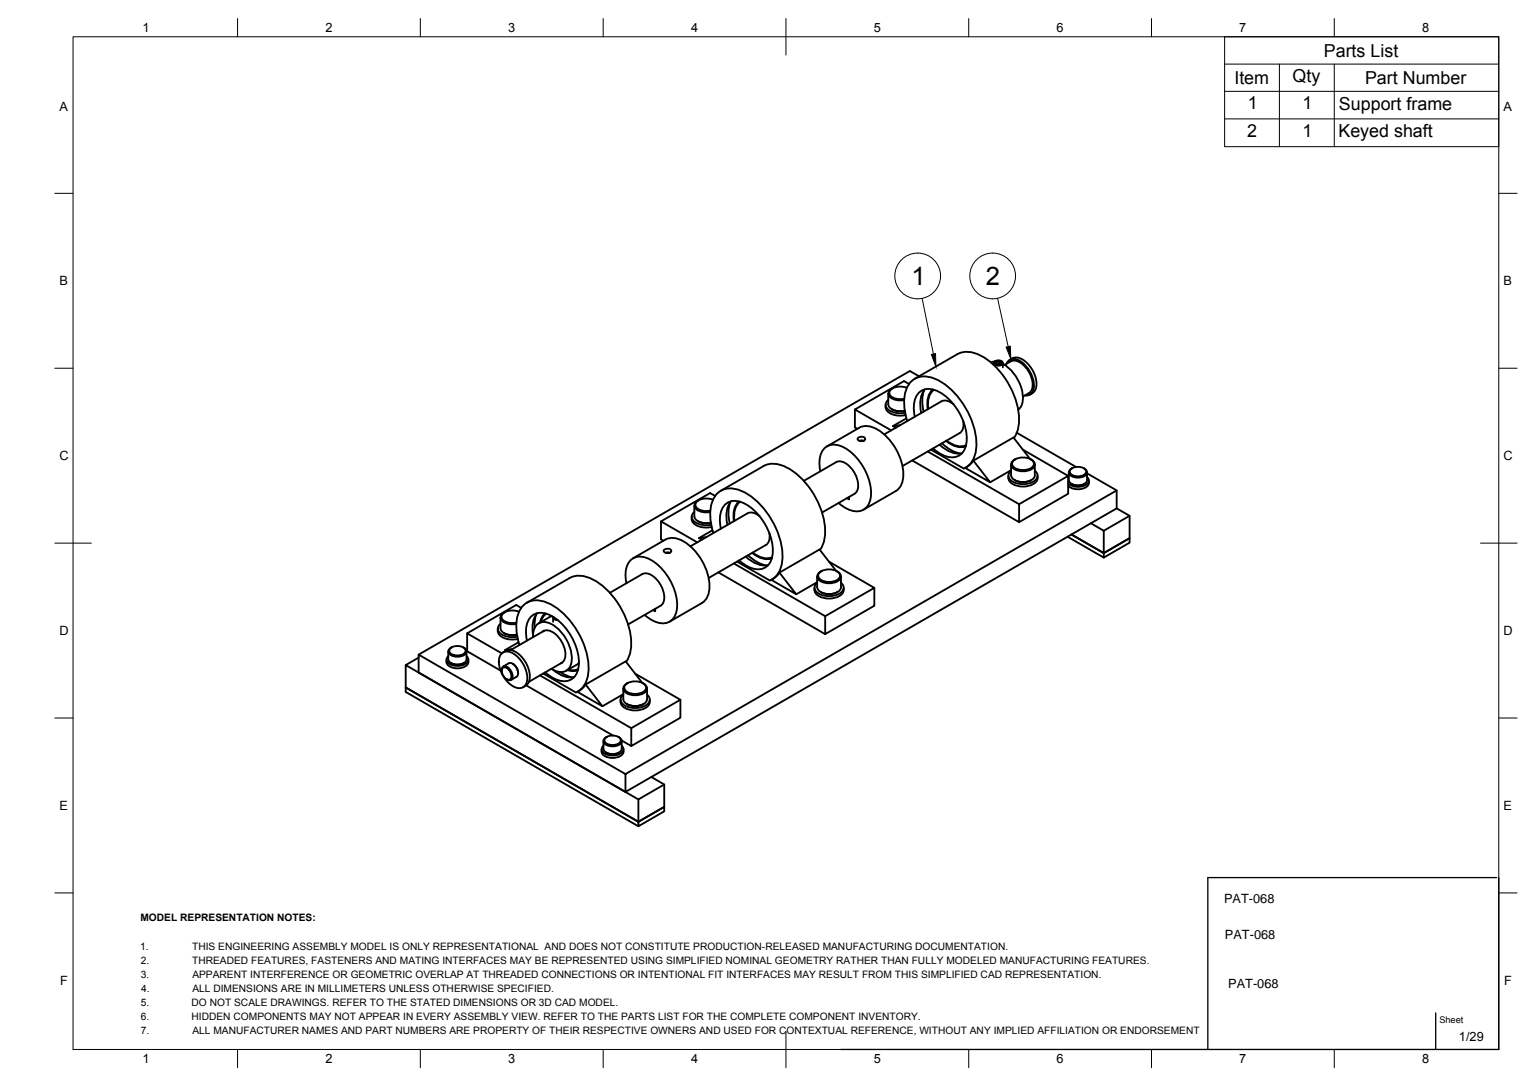
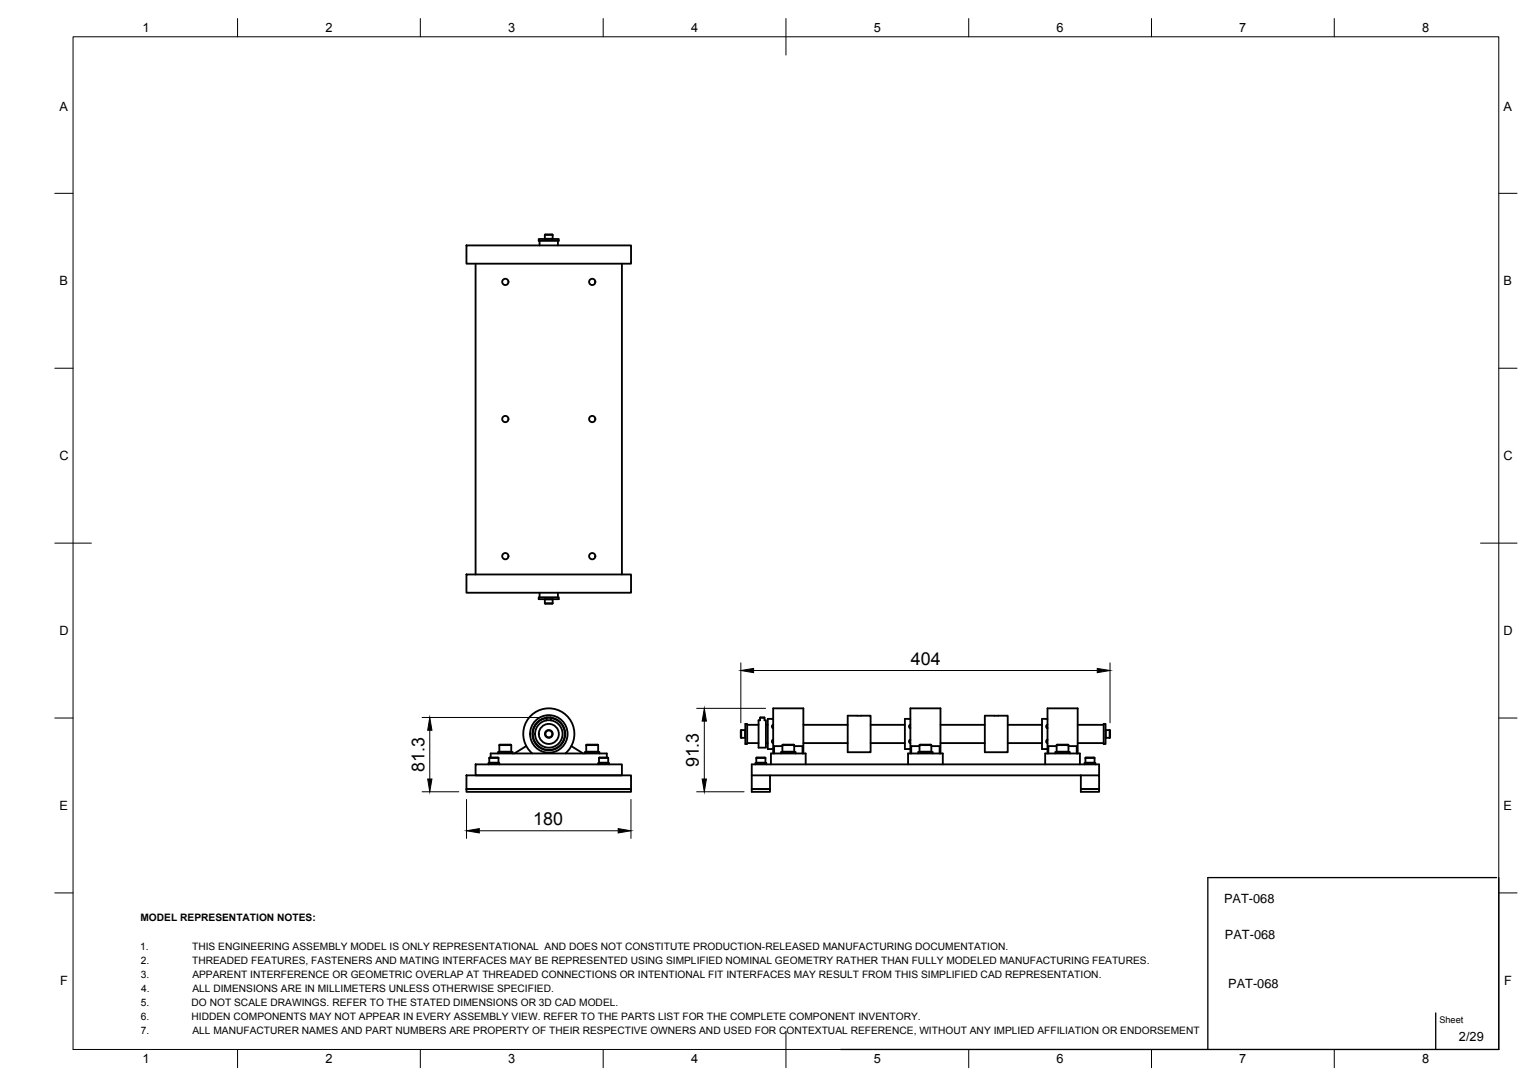
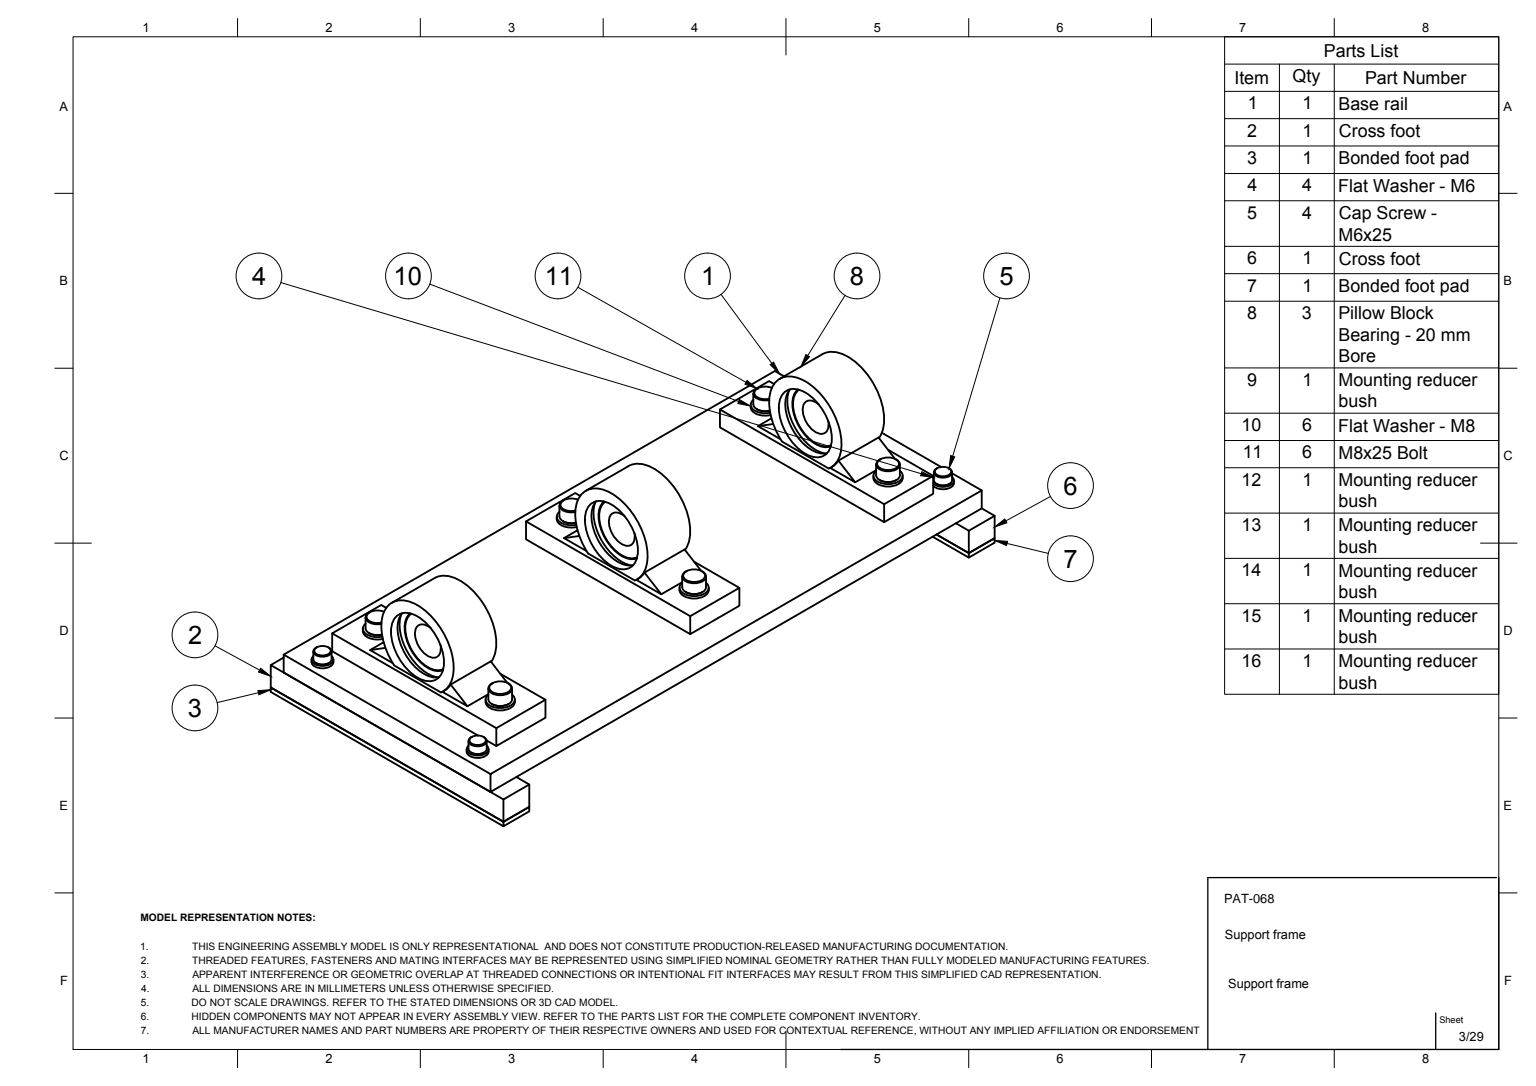
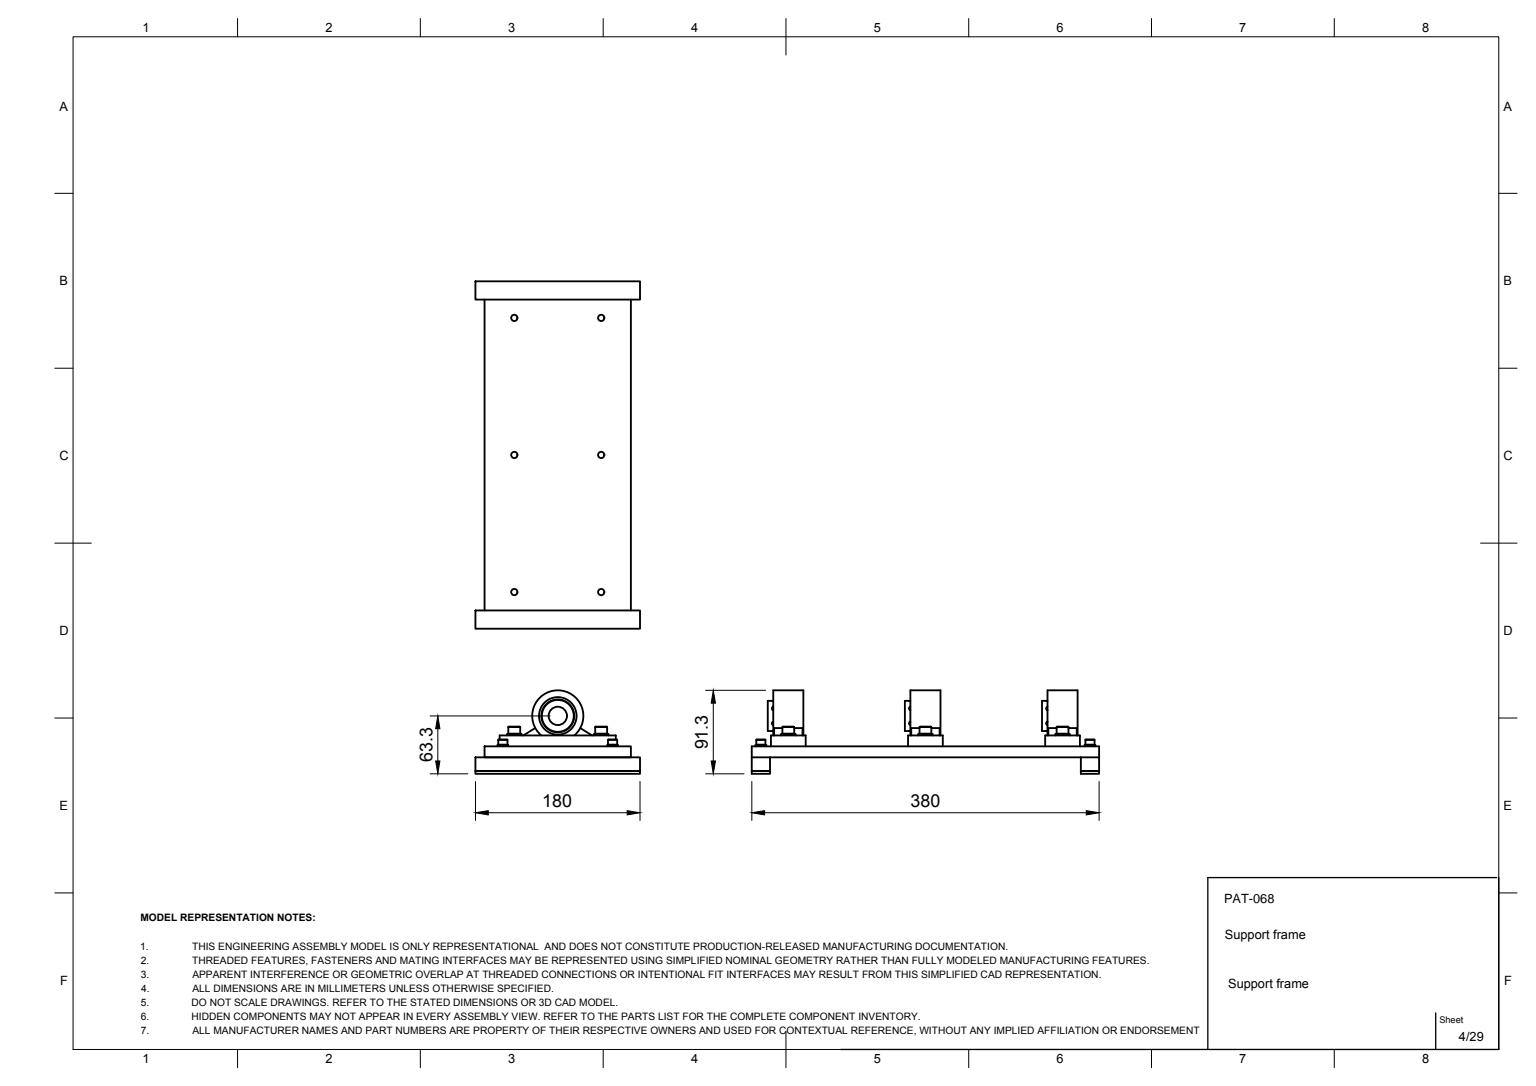
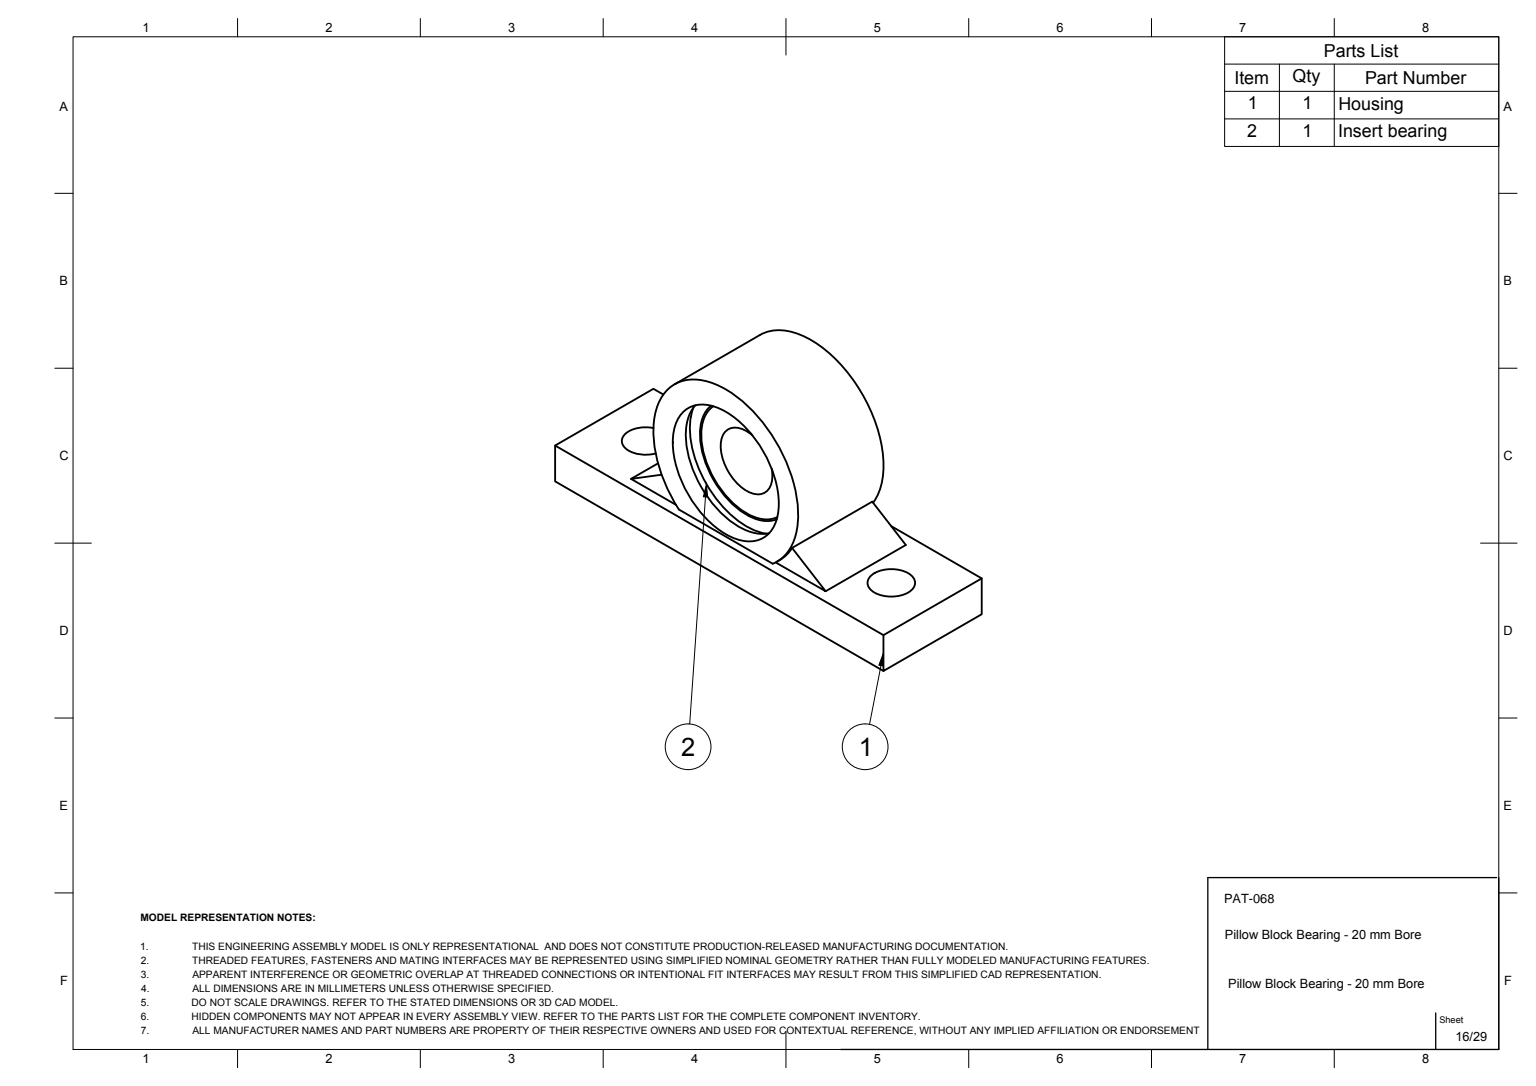
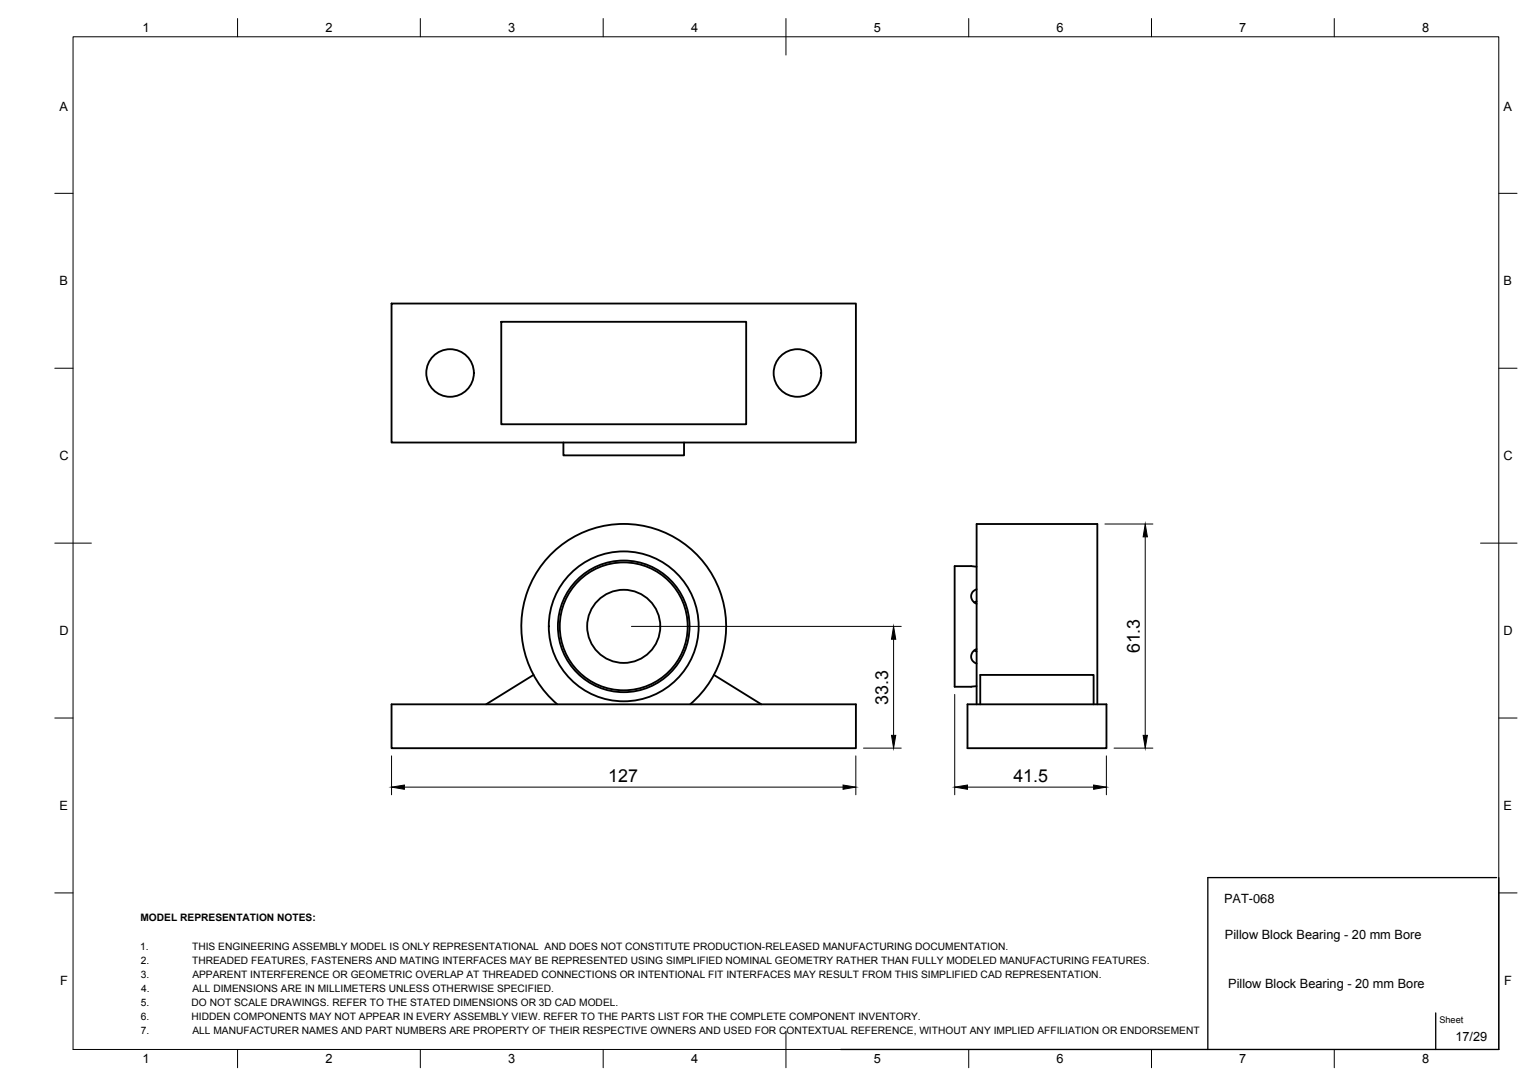
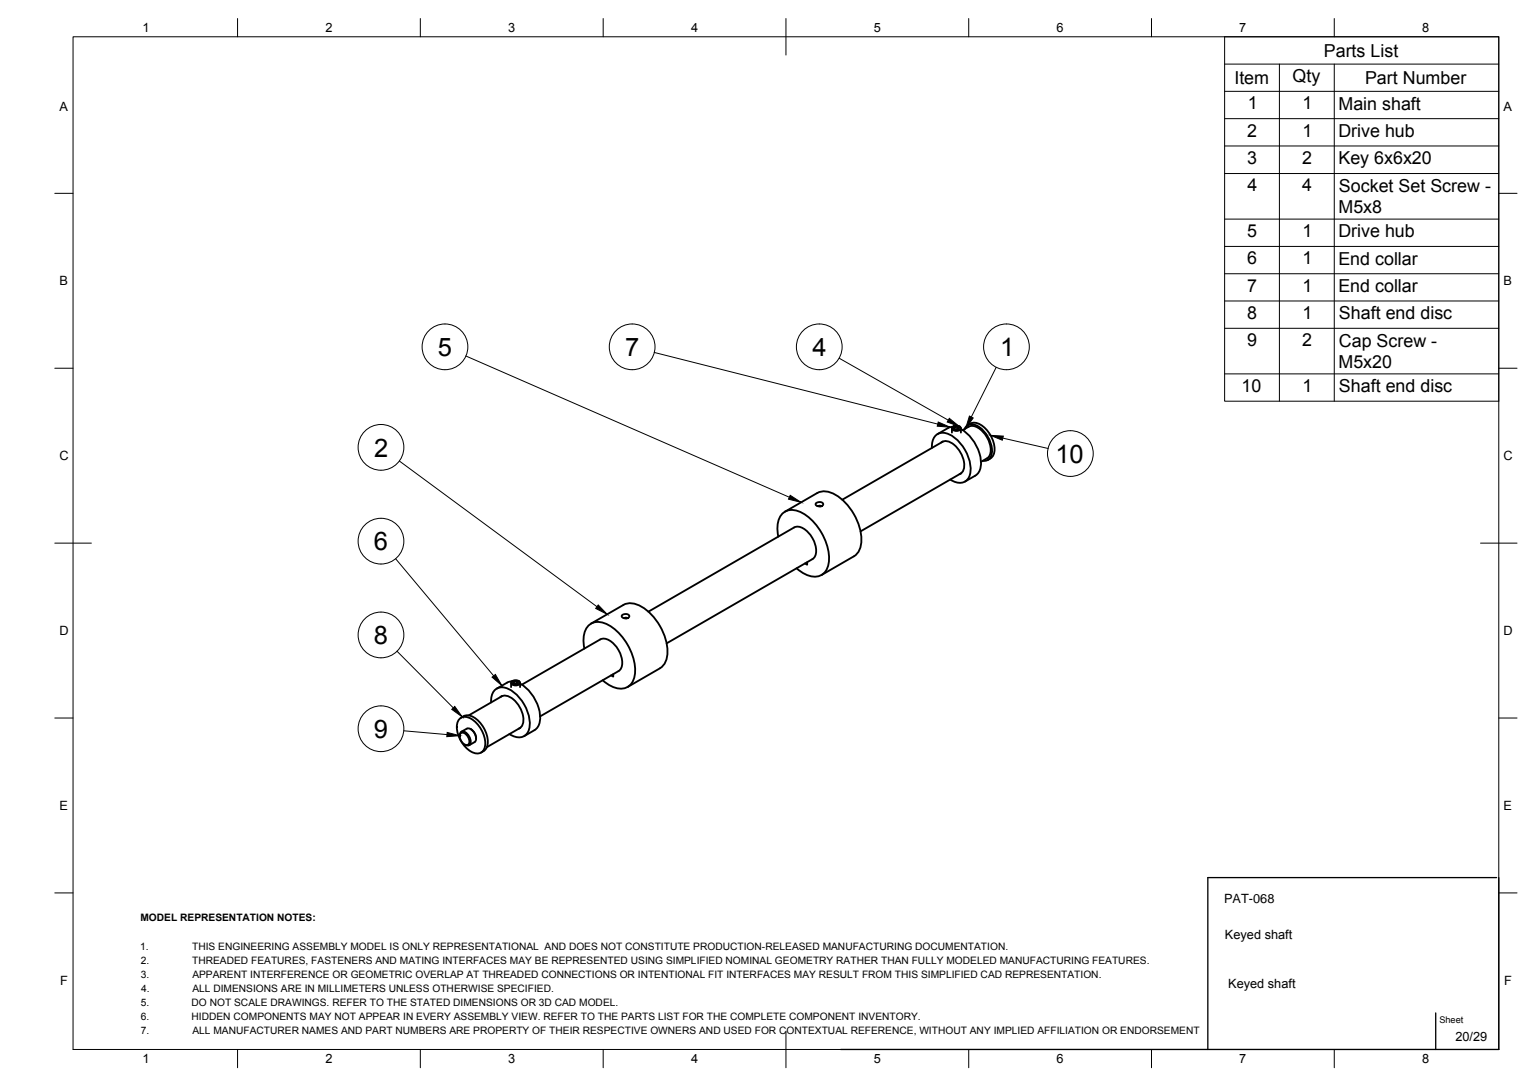
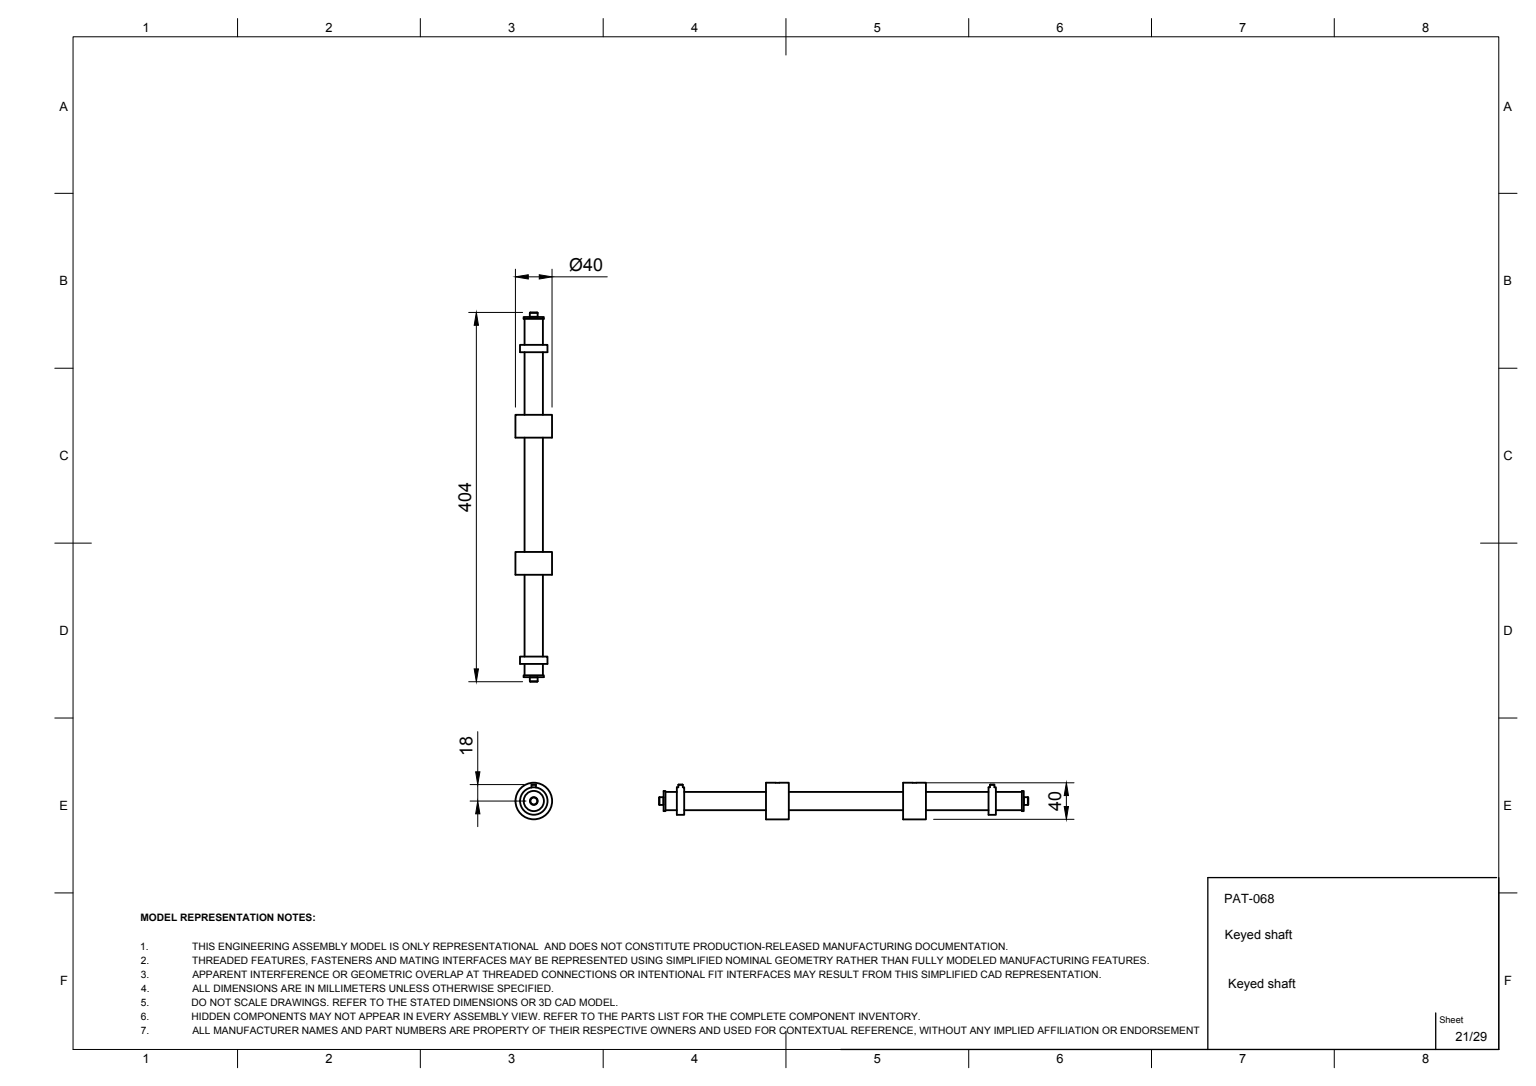
ISO-10303-21;
HEADER;
/* Generated by software containing ST-Developer
 * from STEP Tools, Inc. (www.steptools.com) 
 */

FILE_DESCRIPTION(
/* description */ ('Line shaft on three pillow blocks'),
/* implementation_level */ '2;1');

FILE_NAME(
/* name */ 'PAT-068',
/* time_stamp */ '2026-10-27T10:49:19-07:00',
/* author */ (''),
/* organization */ (''),
/* preprocessor_version */ 'ST-DEVELOPER v20.2',
/* originating_system */ 'Autodesk Translation Framework v15.17.0.0',
/* authorisation */ '');

FILE_SCHEMA (('AUTOMOTIVE_DESIGN { 1 0 10303 214 3 1 1 }'));
ENDSEC;

DATA;
#10=MECHANICAL_DESIGN_GEOMETRIC_PRESENTATION_REPRESENTATION('',(#338,#339,
#340,#341,#342,#343,#344,#345,#346,#347,#348,#349,#350,#351,#352,#353,#354,
#355,#356,#357,#358,#359,#360,#361,#362,#363,#364,#365),#8377);
#11=ITEM_DEFINED_TRANSFORMATION($,$,#4826,#4895);
#12=ITEM_DEFINED_TRANSFORMATION($,$,#4867,#4896);
#13=ITEM_DEFINED_TRANSFORMATION($,$,#4655,#4930);
#14=ITEM_DEFINED_TRANSFORMATION($,$,#4692,#4931);
#15=ITEM_DEFINED_TRANSFORMATION($,$,#4707,#4932);
#16=ITEM_DEFINED_TRANSFORMATION($,$,#4714,#4933);
#17=ITEM_DEFINED_TRANSFORMATION($,$,#4729,#4934);
#18=ITEM_DEFINED_TRANSFORMATION($,$,#4736,#4935);
#19=ITEM_DEFINED_TRANSFORMATION($,$,#4745,#4936);
#20=ITEM_DEFINED_TRANSFORMATION($,$,#4754,#4937);
#21=ITEM_DEFINED_TRANSFORMATION($,$,#4763,#4938);
#22=ITEM_DEFINED_TRANSFORMATION($,$,#4772,#4939);
#23=ITEM_DEFINED_TRANSFORMATION($,$,#4781,#4940);
#24=ITEM_DEFINED_TRANSFORMATION($,$,#4790,#4941);
#25=ITEM_DEFINED_TRANSFORMATION($,$,#4799,#4942);
#26=ITEM_DEFINED_TRANSFORMATION($,$,#4790,#4943);
#27=ITEM_DEFINED_TRANSFORMATION($,$,#4799,#4944);
#28=ITEM_DEFINED_TRANSFORMATION($,$,#4790,#4945);
#29=ITEM_DEFINED_TRANSFORMATION($,$,#4799,#4946);
#30=ITEM_DEFINED_TRANSFORMATION($,$,#4790,#4947);
#31=ITEM_DEFINED_TRANSFORMATION($,$,#4799,#4948);
#32=ITEM_DEFINED_TRANSFORMATION($,$,#4825,#4949);
#33=ITEM_DEFINED_TRANSFORMATION($,$,#4897,#4950);
#34=ITEM_DEFINED_TRANSFORMATION($,$,#4906,#4951);
#35=ITEM_DEFINED_TRANSFORMATION($,$,#4897,#4952);
#36=ITEM_DEFINED_TRANSFORMATION($,$,#4906,#4953);
#37=ITEM_DEFINED_TRANSFORMATION($,$,#4825,#4954);
#38=ITEM_DEFINED_TRANSFORMATION($,$,#4897,#4955);
#39=ITEM_DEFINED_TRANSFORMATION($,$,#4906,#4956);
#40=ITEM_DEFINED_TRANSFORMATION($,$,#4897,#4957);
#41=ITEM_DEFINED_TRANSFORMATION($,$,#4906,#4958);
#42=ITEM_DEFINED_TRANSFORMATION($,$,#4825,#4959);
#43=ITEM_DEFINED_TRANSFORMATION($,$,#4897,#4960);
#44=ITEM_DEFINED_TRANSFORMATION($,$,#4906,#4961);
#45=ITEM_DEFINED_TRANSFORMATION($,$,#4897,#4962);
#46=ITEM_DEFINED_TRANSFORMATION($,$,#4906,#4963);
#47=ITEM_DEFINED_TRANSFORMATION($,$,#4965,#5131);
#48=ITEM_DEFINED_TRANSFORMATION($,$,#4993,#5132);
#49=ITEM_DEFINED_TRANSFORMATION($,$,#5011,#5133);
#50=ITEM_DEFINED_TRANSFORMATION($,$,#5029,#5134);
#51=ITEM_DEFINED_TRANSFORMATION($,$,#5044,#5135);
#52=ITEM_DEFINED_TRANSFORMATION($,$,#5059,#5136);
#53=ITEM_DEFINED_TRANSFORMATION($,$,#5068,#5137);
#54=ITEM_DEFINED_TRANSFORMATION($,$,#5077,#5138);
#55=ITEM_DEFINED_TRANSFORMATION($,$,#5088,#5139);
#56=ITEM_DEFINED_TRANSFORMATION($,$,#5077,#5140);
#57=ITEM_DEFINED_TRANSFORMATION($,$,#5088,#5141);
#58=ITEM_DEFINED_TRANSFORMATION($,$,#5088,#5142);
#59=ITEM_DEFINED_TRANSFORMATION($,$,#5088,#5143);
#60=ITEM_DEFINED_TRANSFORMATION($,$,#5105,#5144);
#61=ITEM_DEFINED_TRANSFORMATION($,$,#5105,#5145);
#62=ITEM_DEFINED_TRANSFORMATION($,$,#4654,#5146);
#63=ITEM_DEFINED_TRANSFORMATION($,$,#4964,#5147);
#64=(
REPRESENTATION_RELATIONSHIP($,$,#8513,#8512)
REPRESENTATION_RELATIONSHIP_WITH_TRANSFORMATION(#11)
SHAPE_REPRESENTATION_RELATIONSHIP()
);
#65=(
REPRESENTATION_RELATIONSHIP($,$,#8514,#8512)
REPRESENTATION_RELATIONSHIP_WITH_TRANSFORMATION(#12)
SHAPE_REPRESENTATION_RELATIONSHIP()
);
#66=(
REPRESENTATION_RELATIONSHIP($,$,#8499,#8498)
REPRESENTATION_RELATIONSHIP_WITH_TRANSFORMATION(#13)
SHAPE_REPRESENTATION_RELATIONSHIP()
);
#67=(
REPRESENTATION_RELATIONSHIP($,$,#8500,#8498)
REPRESENTATION_RELATIONSHIP_WITH_TRANSFORMATION(#14)
SHAPE_REPRESENTATION_RELATIONSHIP()
);
#68=(
REPRESENTATION_RELATIONSHIP($,$,#8501,#8498)
REPRESENTATION_RELATIONSHIP_WITH_TRANSFORMATION(#15)
SHAPE_REPRESENTATION_RELATIONSHIP()
);
#69=(
REPRESENTATION_RELATIONSHIP($,$,#8502,#8498)
REPRESENTATION_RELATIONSHIP_WITH_TRANSFORMATION(#16)
SHAPE_REPRESENTATION_RELATIONSHIP()
);
#70=(
REPRESENTATION_RELATIONSHIP($,$,#8503,#8498)
REPRESENTATION_RELATIONSHIP_WITH_TRANSFORMATION(#17)
SHAPE_REPRESENTATION_RELATIONSHIP()
);
#71=(
REPRESENTATION_RELATIONSHIP($,$,#8504,#8498)
REPRESENTATION_RELATIONSHIP_WITH_TRANSFORMATION(#18)
SHAPE_REPRESENTATION_RELATIONSHIP()
);
#72=(
REPRESENTATION_RELATIONSHIP($,$,#8505,#8498)
REPRESENTATION_RELATIONSHIP_WITH_TRANSFORMATION(#19)
SHAPE_REPRESENTATION_RELATIONSHIP()
);
#73=(
REPRESENTATION_RELATIONSHIP($,$,#8506,#8498)
REPRESENTATION_RELATIONSHIP_WITH_TRANSFORMATION(#20)
SHAPE_REPRESENTATION_RELATIONSHIP()
);
#74=(
REPRESENTATION_RELATIONSHIP($,$,#8507,#8498)
REPRESENTATION_RELATIONSHIP_WITH_TRANSFORMATION(#21)
SHAPE_REPRESENTATION_RELATIONSHIP()
);
#75=(
REPRESENTATION_RELATIONSHIP($,$,#8508,#8498)
REPRESENTATION_RELATIONSHIP_WITH_TRANSFORMATION(#22)
SHAPE_REPRESENTATION_RELATIONSHIP()
);
#76=(
REPRESENTATION_RELATIONSHIP($,$,#8509,#8498)
REPRESENTATION_RELATIONSHIP_WITH_TRANSFORMATION(#23)
SHAPE_REPRESENTATION_RELATIONSHIP()
);
#77=(
REPRESENTATION_RELATIONSHIP($,$,#8510,#8498)
REPRESENTATION_RELATIONSHIP_WITH_TRANSFORMATION(#24)
SHAPE_REPRESENTATION_RELATIONSHIP()
);
#78=(
REPRESENTATION_RELATIONSHIP($,$,#8511,#8498)
REPRESENTATION_RELATIONSHIP_WITH_TRANSFORMATION(#25)
SHAPE_REPRESENTATION_RELATIONSHIP()
);
#79=(
REPRESENTATION_RELATIONSHIP($,$,#8510,#8498)
REPRESENTATION_RELATIONSHIP_WITH_TRANSFORMATION(#26)
SHAPE_REPRESENTATION_RELATIONSHIP()
);
#80=(
REPRESENTATION_RELATIONSHIP($,$,#8511,#8498)
REPRESENTATION_RELATIONSHIP_WITH_TRANSFORMATION(#27)
SHAPE_REPRESENTATION_RELATIONSHIP()
);
#81=(
REPRESENTATION_RELATIONSHIP($,$,#8510,#8498)
REPRESENTATION_RELATIONSHIP_WITH_TRANSFORMATION(#28)
SHAPE_REPRESENTATION_RELATIONSHIP()
);
#82=(
REPRESENTATION_RELATIONSHIP($,$,#8511,#8498)
REPRESENTATION_RELATIONSHIP_WITH_TRANSFORMATION(#29)
SHAPE_REPRESENTATION_RELATIONSHIP()
);
#83=(
REPRESENTATION_RELATIONSHIP($,$,#8510,#8498)
REPRESENTATION_RELATIONSHIP_WITH_TRANSFORMATION(#30)
SHAPE_REPRESENTATION_RELATIONSHIP()
);
#84=(
REPRESENTATION_RELATIONSHIP($,$,#8511,#8498)
REPRESENTATION_RELATIONSHIP_WITH_TRANSFORMATION(#31)
SHAPE_REPRESENTATION_RELATIONSHIP()
);
#85=(
REPRESENTATION_RELATIONSHIP($,$,#8512,#8498)
REPRESENTATION_RELATIONSHIP_WITH_TRANSFORMATION(#32)
SHAPE_REPRESENTATION_RELATIONSHIP()
);
#86=(
REPRESENTATION_RELATIONSHIP($,$,#8515,#8498)
REPRESENTATION_RELATIONSHIP_WITH_TRANSFORMATION(#33)
SHAPE_REPRESENTATION_RELATIONSHIP()
);
#87=(
REPRESENTATION_RELATIONSHIP($,$,#8516,#8498)
REPRESENTATION_RELATIONSHIP_WITH_TRANSFORMATION(#34)
SHAPE_REPRESENTATION_RELATIONSHIP()
);
#88=(
REPRESENTATION_RELATIONSHIP($,$,#8515,#8498)
REPRESENTATION_RELATIONSHIP_WITH_TRANSFORMATION(#35)
SHAPE_REPRESENTATION_RELATIONSHIP()
);
#89=(
REPRESENTATION_RELATIONSHIP($,$,#8516,#8498)
REPRESENTATION_RELATIONSHIP_WITH_TRANSFORMATION(#36)
SHAPE_REPRESENTATION_RELATIONSHIP()
);
#90=(
REPRESENTATION_RELATIONSHIP($,$,#8512,#8498)
REPRESENTATION_RELATIONSHIP_WITH_TRANSFORMATION(#37)
SHAPE_REPRESENTATION_RELATIONSHIP()
);
#91=(
REPRESENTATION_RELATIONSHIP($,$,#8515,#8498)
REPRESENTATION_RELATIONSHIP_WITH_TRANSFORMATION(#38)
SHAPE_REPRESENTATION_RELATIONSHIP()
);
#92=(
REPRESENTATION_RELATIONSHIP($,$,#8516,#8498)
REPRESENTATION_RELATIONSHIP_WITH_TRANSFORMATION(#39)
SHAPE_REPRESENTATION_RELATIONSHIP()
);
#93=(
REPRESENTATION_RELATIONSHIP($,$,#8515,#8498)
REPRESENTATION_RELATIONSHIP_WITH_TRANSFORMATION(#40)
SHAPE_REPRESENTATION_RELATIONSHIP()
);
#94=(
REPRESENTATION_RELATIONSHIP($,$,#8516,#8498)
REPRESENTATION_RELATIONSHIP_WITH_TRANSFORMATION(#41)
SHAPE_REPRESENTATION_RELATIONSHIP()
);
#95=(
REPRESENTATION_RELATIONSHIP($,$,#8512,#8498)
REPRESENTATION_RELATIONSHIP_WITH_TRANSFORMATION(#42)
SHAPE_REPRESENTATION_RELATIONSHIP()
);
#96=(
REPRESENTATION_RELATIONSHIP($,$,#8515,#8498)
REPRESENTATION_RELATIONSHIP_WITH_TRANSFORMATION(#43)
SHAPE_REPRESENTATION_RELATIONSHIP()
);
#97=(
REPRESENTATION_RELATIONSHIP($,$,#8516,#8498)
REPRESENTATION_RELATIONSHIP_WITH_TRANSFORMATION(#44)
SHAPE_REPRESENTATION_RELATIONSHIP()
);
#98=(
REPRESENTATION_RELATIONSHIP($,$,#8515,#8498)
REPRESENTATION_RELATIONSHIP_WITH_TRANSFORMATION(#45)
SHAPE_REPRESENTATION_RELATIONSHIP()
);
#99=(
REPRESENTATION_RELATIONSHIP($,$,#8516,#8498)
REPRESENTATION_RELATIONSHIP_WITH_TRANSFORMATION(#46)
SHAPE_REPRESENTATION_RELATIONSHIP()
);
#100=(
REPRESENTATION_RELATIONSHIP($,$,#8518,#8517)
REPRESENTATION_RELATIONSHIP_WITH_TRANSFORMATION(#47)
SHAPE_REPRESENTATION_RELATIONSHIP()
);
#101=(
REPRESENTATION_RELATIONSHIP($,$,#8519,#8517)
REPRESENTATION_RELATIONSHIP_WITH_TRANSFORMATION(#48)
SHAPE_REPRESENTATION_RELATIONSHIP()
);
#102=(
REPRESENTATION_RELATIONSHIP($,$,#8520,#8517)
REPRESENTATION_RELATIONSHIP_WITH_TRANSFORMATION(#49)
SHAPE_REPRESENTATION_RELATIONSHIP()
);
#103=(
REPRESENTATION_RELATIONSHIP($,$,#8521,#8517)
REPRESENTATION_RELATIONSHIP_WITH_TRANSFORMATION(#50)
SHAPE_REPRESENTATION_RELATIONSHIP()
);
#104=(
REPRESENTATION_RELATIONSHIP($,$,#8522,#8517)
REPRESENTATION_RELATIONSHIP_WITH_TRANSFORMATION(#51)
SHAPE_REPRESENTATION_RELATIONSHIP()
);
#105=(
REPRESENTATION_RELATIONSHIP($,$,#8523,#8517)
REPRESENTATION_RELATIONSHIP_WITH_TRANSFORMATION(#52)
SHAPE_REPRESENTATION_RELATIONSHIP()
);
#106=(
REPRESENTATION_RELATIONSHIP($,$,#8524,#8517)
REPRESENTATION_RELATIONSHIP_WITH_TRANSFORMATION(#53)
SHAPE_REPRESENTATION_RELATIONSHIP()
);
#107=(
REPRESENTATION_RELATIONSHIP($,$,#8525,#8517)
REPRESENTATION_RELATIONSHIP_WITH_TRANSFORMATION(#54)
SHAPE_REPRESENTATION_RELATIONSHIP()
);
#108=(
REPRESENTATION_RELATIONSHIP($,$,#8526,#8517)
REPRESENTATION_RELATIONSHIP_WITH_TRANSFORMATION(#55)
SHAPE_REPRESENTATION_RELATIONSHIP()
);
#109=(
REPRESENTATION_RELATIONSHIP($,$,#8525,#8517)
REPRESENTATION_RELATIONSHIP_WITH_TRANSFORMATION(#56)
SHAPE_REPRESENTATION_RELATIONSHIP()
);
#110=(
REPRESENTATION_RELATIONSHIP($,$,#8526,#8517)
REPRESENTATION_RELATIONSHIP_WITH_TRANSFORMATION(#57)
SHAPE_REPRESENTATION_RELATIONSHIP()
);
#111=(
REPRESENTATION_RELATIONSHIP($,$,#8526,#8517)
REPRESENTATION_RELATIONSHIP_WITH_TRANSFORMATION(#58)
SHAPE_REPRESENTATION_RELATIONSHIP()
);
#112=(
REPRESENTATION_RELATIONSHIP($,$,#8526,#8517)
REPRESENTATION_RELATIONSHIP_WITH_TRANSFORMATION(#59)
SHAPE_REPRESENTATION_RELATIONSHIP()
);
#113=(
REPRESENTATION_RELATIONSHIP($,$,#8527,#8517)
REPRESENTATION_RELATIONSHIP_WITH_TRANSFORMATION(#60)
SHAPE_REPRESENTATION_RELATIONSHIP()
);
#114=(
REPRESENTATION_RELATIONSHIP($,$,#8527,#8517)
REPRESENTATION_RELATIONSHIP_WITH_TRANSFORMATION(#61)
SHAPE_REPRESENTATION_RELATIONSHIP()
);
#115=(
REPRESENTATION_RELATIONSHIP($,$,#8498,#8497)
REPRESENTATION_RELATIONSHIP_WITH_TRANSFORMATION(#62)
SHAPE_REPRESENTATION_RELATIONSHIP()
);
#116=(
REPRESENTATION_RELATIONSHIP($,$,#8517,#8497)
REPRESENTATION_RELATIONSHIP_WITH_TRANSFORMATION(#63)
SHAPE_REPRESENTATION_RELATIONSHIP()
);
#117=CONTEXT_DEPENDENT_SHAPE_REPRESENTATION(#64,#8431);
#118=CONTEXT_DEPENDENT_SHAPE_REPRESENTATION(#65,#8432);
#119=CONTEXT_DEPENDENT_SHAPE_REPRESENTATION(#66,#8435);
#120=CONTEXT_DEPENDENT_SHAPE_REPRESENTATION(#67,#8436);
#121=CONTEXT_DEPENDENT_SHAPE_REPRESENTATION(#68,#8437);
#122=CONTEXT_DEPENDENT_SHAPE_REPRESENTATION(#69,#8438);
#123=CONTEXT_DEPENDENT_SHAPE_REPRESENTATION(#70,#8439);
#124=CONTEXT_DEPENDENT_SHAPE_REPRESENTATION(#71,#8440);
#125=CONTEXT_DEPENDENT_SHAPE_REPRESENTATION(#72,#8441);
#126=CONTEXT_DEPENDENT_SHAPE_REPRESENTATION(#73,#8442);
#127=CONTEXT_DEPENDENT_SHAPE_REPRESENTATION(#74,#8443);
#128=CONTEXT_DEPENDENT_SHAPE_REPRESENTATION(#75,#8444);
#129=CONTEXT_DEPENDENT_SHAPE_REPRESENTATION(#76,#8445);
#130=CONTEXT_DEPENDENT_SHAPE_REPRESENTATION(#77,#8446);
#131=CONTEXT_DEPENDENT_SHAPE_REPRESENTATION(#78,#8447);
#132=CONTEXT_DEPENDENT_SHAPE_REPRESENTATION(#79,#8448);
#133=CONTEXT_DEPENDENT_SHAPE_REPRESENTATION(#80,#8449);
#134=CONTEXT_DEPENDENT_SHAPE_REPRESENTATION(#81,#8450);
#135=CONTEXT_DEPENDENT_SHAPE_REPRESENTATION(#82,#8451);
#136=CONTEXT_DEPENDENT_SHAPE_REPRESENTATION(#83,#8452);
#137=CONTEXT_DEPENDENT_SHAPE_REPRESENTATION(#84,#8453);
#138=CONTEXT_DEPENDENT_SHAPE_REPRESENTATION(#85,#8454);
#139=CONTEXT_DEPENDENT_SHAPE_REPRESENTATION(#86,#8455);
#140=CONTEXT_DEPENDENT_SHAPE_REPRESENTATION(#87,#8456);
#141=CONTEXT_DEPENDENT_SHAPE_REPRESENTATION(#88,#8457);
#142=CONTEXT_DEPENDENT_SHAPE_REPRESENTATION(#89,#8458);
#143=CONTEXT_DEPENDENT_SHAPE_REPRESENTATION(#90,#8459);
#144=CONTEXT_DEPENDENT_SHAPE_REPRESENTATION(#91,#8460);
#145=CONTEXT_DEPENDENT_SHAPE_REPRESENTATION(#92,#8461);
#146=CONTEXT_DEPENDENT_SHAPE_REPRESENTATION(#93,#8462);
#147=CONTEXT_DEPENDENT_SHAPE_REPRESENTATION(#94,#8463);
#148=CONTEXT_DEPENDENT_SHAPE_REPRESENTATION(#95,#8464);
#149=CONTEXT_DEPENDENT_SHAPE_REPRESENTATION(#96,#8465);
#150=CONTEXT_DEPENDENT_SHAPE_REPRESENTATION(#97,#8466);
#151=CONTEXT_DEPENDENT_SHAPE_REPRESENTATION(#98,#8467);
#152=CONTEXT_DEPENDENT_SHAPE_REPRESENTATION(#99,#8468);
#153=CONTEXT_DEPENDENT_SHAPE_REPRESENTATION(#100,#8480);
#154=CONTEXT_DEPENDENT_SHAPE_REPRESENTATION(#101,#8481);
#155=CONTEXT_DEPENDENT_SHAPE_REPRESENTATION(#102,#8482);
#156=CONTEXT_DEPENDENT_SHAPE_REPRESENTATION(#103,#8483);
#157=CONTEXT_DEPENDENT_SHAPE_REPRESENTATION(#104,#8484);
#158=CONTEXT_DEPENDENT_SHAPE_REPRESENTATION(#105,#8485);
#159=CONTEXT_DEPENDENT_SHAPE_REPRESENTATION(#106,#8486);
#160=CONTEXT_DEPENDENT_SHAPE_REPRESENTATION(#107,#8487);
#161=CONTEXT_DEPENDENT_SHAPE_REPRESENTATION(#108,#8488);
#162=CONTEXT_DEPENDENT_SHAPE_REPRESENTATION(#109,#8489);
#163=CONTEXT_DEPENDENT_SHAPE_REPRESENTATION(#110,#8490);
#164=CONTEXT_DEPENDENT_SHAPE_REPRESENTATION(#111,#8491);
#165=CONTEXT_DEPENDENT_SHAPE_REPRESENTATION(#112,#8492);
#166=CONTEXT_DEPENDENT_SHAPE_REPRESENTATION(#113,#8493);
#167=CONTEXT_DEPENDENT_SHAPE_REPRESENTATION(#114,#8494);
#168=CONTEXT_DEPENDENT_SHAPE_REPRESENTATION(#115,#8495);
#169=CONTEXT_DEPENDENT_SHAPE_REPRESENTATION(#116,#8496);
#170=NEXT_ASSEMBLY_USAGE_OCCURRENCE('Housing:1','Housing:1','Housing:1',
#8544,#8545,'Housing:1');
#171=NEXT_ASSEMBLY_USAGE_OCCURRENCE('Insert bearing:1',
'Insert bearing:1','Insert bearing:1',#8544,#8546,'Insert bearing:1');
#172=NEXT_ASSEMBLY_USAGE_OCCURRENCE('Base rail:1','Base rail:1',
'Base rail:1',#8530,#8531,'Base rail:1');
#173=NEXT_ASSEMBLY_USAGE_OCCURRENCE('Cross foot:1','Cross foot:1',
'Cross foot:1',#8530,#8532,'Cross foot:1');
#174=NEXT_ASSEMBLY_USAGE_OCCURRENCE('Bonded foot pad:1',
'Bonded foot pad:1','Bonded foot pad:1',#8530,#8533,'Bonded foot pad:1');
#175=NEXT_ASSEMBLY_USAGE_OCCURRENCE('Cross foot (1):1',
'Cross foot (1):1','Cross foot (1):1',#8530,#8534,'Cross foot (1):1');
#176=NEXT_ASSEMBLY_USAGE_OCCURRENCE('Bonded foot pad (1):1',
'Bonded foot pad (1):1','Bonded foot pad (1):1',#8530,#8535,
'Bonded foot pad (1):1');
#177=NEXT_ASSEMBLY_USAGE_OCCURRENCE('Mounting reducer bush:1',
'Mounting reducer bush:1','Mounting reducer bush:1',#8530,#8536,
'Mounting reducer bush:1');
#178=NEXT_ASSEMBLY_USAGE_OCCURRENCE('Mounting reducer bush (1):1',
'Mounting reducer bush (1):1','Mounting reducer bush (1):1',#8530,#8537,
'Mounting reducer bush (1):1');
#179=NEXT_ASSEMBLY_USAGE_OCCURRENCE('Mounting reducer bush (2):1',
'Mounting reducer bush (2):1','Mounting reducer bush (2):1',#8530,#8538,
'Mounting reducer bush (2):1');
#180=NEXT_ASSEMBLY_USAGE_OCCURRENCE('Mounting reducer bush (3):1',
'Mounting reducer bush (3):1','Mounting reducer bush (3):1',#8530,#8539,
'Mounting reducer bush (3):1');
#181=NEXT_ASSEMBLY_USAGE_OCCURRENCE('Mounting reducer bush (4):1',
'Mounting reducer bush (4):1','Mounting reducer bush (4):1',#8530,#8540,
'Mounting reducer bush (4):1');
#182=NEXT_ASSEMBLY_USAGE_OCCURRENCE('Mounting reducer bush (5):1',
'Mounting reducer bush (5):1','Mounting reducer bush (5):1',#8530,#8541,
'Mounting reducer bush (5):1');
#183=NEXT_ASSEMBLY_USAGE_OCCURRENCE('Flat Washer - M6:2',
'Flat Washer - M6:2','Flat Washer - M6:2',#8530,#8542,
'Flat Washer - M6:2');
#184=NEXT_ASSEMBLY_USAGE_OCCURRENCE('Cap Screw - M6x25:2',
'Cap Screw - M6x25:2','Cap Screw - M6x25:2',#8530,#8543,
'Cap Screw - M6x25:2');
#185=NEXT_ASSEMBLY_USAGE_OCCURRENCE('Flat Washer - M6:3',
'Flat Washer - M6:3','Flat Washer - M6:3',#8530,#8542,
'Flat Washer - M6:3');
#186=NEXT_ASSEMBLY_USAGE_OCCURRENCE('Cap Screw - M6x25:3',
'Cap Screw - M6x25:3','Cap Screw - M6x25:3',#8530,#8543,
'Cap Screw - M6x25:3');
#187=NEXT_ASSEMBLY_USAGE_OCCURRENCE('Flat Washer - M6:4',
'Flat Washer - M6:4','Flat Washer - M6:4',#8530,#8542,
'Flat Washer - M6:4');
#188=NEXT_ASSEMBLY_USAGE_OCCURRENCE('Cap Screw - M6x25:4',
'Cap Screw - M6x25:4','Cap Screw - M6x25:4',#8530,#8543,
'Cap Screw - M6x25:4');
#189=NEXT_ASSEMBLY_USAGE_OCCURRENCE('Flat Washer - M6:5',
'Flat Washer - M6:5','Flat Washer - M6:5',#8530,#8542,
'Flat Washer - M6:5');
#190=NEXT_ASSEMBLY_USAGE_OCCURRENCE('Cap Screw - M6x25:5',
'Cap Screw - M6x25:5','Cap Screw - M6x25:5',#8530,#8543,
'Cap Screw - M6x25:5');
#191=NEXT_ASSEMBLY_USAGE_OCCURRENCE(
'Pillow Block Bearing - 20 mm Bore:2',
'Pillow Block Bearing - 20 mm Bore:2',
'Pillow Block Bearing - 20 mm Bore:2',#8530,#8544,
'Pillow Block Bearing - 20 mm Bore:2');
#192=NEXT_ASSEMBLY_USAGE_OCCURRENCE('Flat Washer - M8:2',
'Flat Washer - M8:2','Flat Washer - M8:2',#8530,#8547,
'Flat Washer - M8:2');
#193=NEXT_ASSEMBLY_USAGE_OCCURRENCE('M8x25 Bolt:2','M8x25 Bolt:2',
'M8x25 Bolt:2',#8530,#8548,'M8x25 Bolt:2');
#194=NEXT_ASSEMBLY_USAGE_OCCURRENCE('Flat Washer - M8:3',
'Flat Washer - M8:3','Flat Washer - M8:3',#8530,#8547,
'Flat Washer - M8:3');
#195=NEXT_ASSEMBLY_USAGE_OCCURRENCE('M8x25 Bolt:3','M8x25 Bolt:3',
'M8x25 Bolt:3',#8530,#8548,'M8x25 Bolt:3');
#196=NEXT_ASSEMBLY_USAGE_OCCURRENCE(
'Pillow Block Bearing - 20 mm Bore:3',
'Pillow Block Bearing - 20 mm Bore:3',
'Pillow Block Bearing - 20 mm Bore:3',#8530,#8544,
'Pillow Block Bearing - 20 mm Bore:3');
#197=NEXT_ASSEMBLY_USAGE_OCCURRENCE('Flat Washer - M8:4',
'Flat Washer - M8:4','Flat Washer - M8:4',#8530,#8547,
'Flat Washer - M8:4');
#198=NEXT_ASSEMBLY_USAGE_OCCURRENCE('M8x25 Bolt:4','M8x25 Bolt:4',
'M8x25 Bolt:4',#8530,#8548,'M8x25 Bolt:4');
#199=NEXT_ASSEMBLY_USAGE_OCCURRENCE('Flat Washer - M8:5',
'Flat Washer - M8:5','Flat Washer - M8:5',#8530,#8547,
'Flat Washer - M8:5');
#200=NEXT_ASSEMBLY_USAGE_OCCURRENCE('M8x25 Bolt:5','M8x25 Bolt:5',
'M8x25 Bolt:5',#8530,#8548,'M8x25 Bolt:5');
#201=NEXT_ASSEMBLY_USAGE_OCCURRENCE(
'Pillow Block Bearing - 20 mm Bore:4',
'Pillow Block Bearing - 20 mm Bore:4',
'Pillow Block Bearing - 20 mm Bore:4',#8530,#8544,
'Pillow Block Bearing - 20 mm Bore:4');
#202=NEXT_ASSEMBLY_USAGE_OCCURRENCE('Flat Washer - M8:6',
'Flat Washer - M8:6','Flat Washer - M8:6',#8530,#8547,
'Flat Washer - M8:6');
#203=NEXT_ASSEMBLY_USAGE_OCCURRENCE('M8x25 Bolt:6','M8x25 Bolt:6',
'M8x25 Bolt:6',#8530,#8548,'M8x25 Bolt:6');
#204=NEXT_ASSEMBLY_USAGE_OCCURRENCE('Flat Washer - M8:7',
'Flat Washer - M8:7','Flat Washer - M8:7',#8530,#8547,
'Flat Washer - M8:7');
#205=NEXT_ASSEMBLY_USAGE_OCCURRENCE('M8x25 Bolt:7','M8x25 Bolt:7',
'M8x25 Bolt:7',#8530,#8548,'M8x25 Bolt:7');
#206=NEXT_ASSEMBLY_USAGE_OCCURRENCE('Main shaft:1','Main shaft:1',
'Main shaft:1',#8549,#8550,'Main shaft:1');
#207=NEXT_ASSEMBLY_USAGE_OCCURRENCE('Drive hub:1','Drive hub:1',
'Drive hub:1',#8549,#8551,'Drive hub:1');
#208=NEXT_ASSEMBLY_USAGE_OCCURRENCE('Drive hub (1):1','Drive hub (1):1',
'Drive hub (1):1',#8549,#8552,'Drive hub (1):1');
#209=NEXT_ASSEMBLY_USAGE_OCCURRENCE('End collar:1','End collar:1',
'End collar:1',#8549,#8553,'End collar:1');
#210=NEXT_ASSEMBLY_USAGE_OCCURRENCE('End collar (1):1',
'End collar (1):1','End collar (1):1',#8549,#8554,'End collar (1):1');
#211=NEXT_ASSEMBLY_USAGE_OCCURRENCE('Shaft end disc:1',
'Shaft end disc:1','Shaft end disc:1',#8549,#8555,'Shaft end disc:1');
#212=NEXT_ASSEMBLY_USAGE_OCCURRENCE('Shaft end disc (1):1',
'Shaft end disc (1):1','Shaft end disc (1):1',#8549,#8556,
'Shaft end disc (1):1');
#213=NEXT_ASSEMBLY_USAGE_OCCURRENCE('Key 6x6x20:2','Key 6x6x20:2',
'Key 6x6x20:2',#8549,#8557,'Key 6x6x20:2');
#214=NEXT_ASSEMBLY_USAGE_OCCURRENCE('Socket Set Screw - M5x8:2',
'Socket Set Screw - M5x8:2','Socket Set Screw - M5x8:2',#8549,#8558,
'Socket Set Screw - M5x8:2');
#215=NEXT_ASSEMBLY_USAGE_OCCURRENCE('Key 6x6x20:3','Key 6x6x20:3',
'Key 6x6x20:3',#8549,#8557,'Key 6x6x20:3');
#216=NEXT_ASSEMBLY_USAGE_OCCURRENCE('Socket Set Screw - M5x8:3',
'Socket Set Screw - M5x8:3','Socket Set Screw - M5x8:3',#8549,#8558,
'Socket Set Screw - M5x8:3');
#217=NEXT_ASSEMBLY_USAGE_OCCURRENCE('Socket Set Screw - M5x8:4',
'Socket Set Screw - M5x8:4','Socket Set Screw - M5x8:4',#8549,#8558,
'Socket Set Screw - M5x8:4');
#218=NEXT_ASSEMBLY_USAGE_OCCURRENCE('Socket Set Screw - M5x8:5',
'Socket Set Screw - M5x8:5','Socket Set Screw - M5x8:5',#8549,#8558,
'Socket Set Screw - M5x8:5');
#219=NEXT_ASSEMBLY_USAGE_OCCURRENCE('Cap Screw - M5x20:2',
'Cap Screw - M5x20:2','Cap Screw - M5x20:2',#8549,#8559,
'Cap Screw - M5x20:2');
#220=NEXT_ASSEMBLY_USAGE_OCCURRENCE('Cap Screw - M5x20:3',
'Cap Screw - M5x20:3','Cap Screw - M5x20:3',#8549,#8559,
'Cap Screw - M5x20:3');
#221=NEXT_ASSEMBLY_USAGE_OCCURRENCE('Support frame:1','Support frame:1',
'Support frame:1',#8529,#8530,'Support frame:1');
#222=NEXT_ASSEMBLY_USAGE_OCCURRENCE('Keyed shaft:1','Keyed shaft:1',
'Keyed shaft:1',#8529,#8549,'Keyed shaft:1');
#223=B_SPLINE_CURVE_WITH_KNOTS('',3,(#7015,#7016,#7017,#7018,#7019,#7020,
#7021,#7022,#7023,#7024),.UNSPECIFIED.,.F.,.F.,(4,2,2,2,4),(1.13193471301885,
1.22626174930539,1.32058878559194,1.41491753480854,1.50924628402513),
 .UNSPECIFIED.);
#224=B_SPLINE_CURVE_WITH_KNOTS('',3,(#7026,#7027,#7028,#7029,#7030,#7031,
#7032,#7033,#7034,#7035,#7036,#7037,#7038,#7039,#7040,#7041,#7042,#7043),
 .UNSPECIFIED.,.F.,.F.,(4,2,2,2,2,2,2,2,4),(0.377311571006283,0.471638607292829,
0.565965643579376,0.66029439279597,0.754623142012565,0.84895189122916,0.943280640445754,
1.0376076767323,1.13193471301885),.UNSPECIFIED.);
#225=B_SPLINE_CURVE_WITH_KNOTS('',3,(#7044,#7045,#7046,#7047,#7048,#7049,
#7050,#7051,#7052,#7053),.UNSPECIFIED.,.F.,.F.,(4,2,2,2,4),(1.50924628402513,
1.60357503324173,1.69790378245832,1.79223081874487,1.88655785503141),
 .UNSPECIFIED.);
#226=B_SPLINE_CURVE_WITH_KNOTS('',3,(#7056,#7057,#7058,#7059,#7060,#7061,
#7062,#7063,#7064,#7065,#7066,#7067,#7068,#7069,#7070,#7071,#7072,#7073,
#7074,#7075,#7076,#7077,#7078,#7079,#7080,#7081,#7082,#7083,#7084,#7085,
#7086,#7087,#7088,#7089),.UNSPECIFIED.,.T.,.F.,(4,2,2,2,2,2,2,2,2,2,2,2,
2,2,2,2,4),(0.,0.0946120580087934,0.189224116017587,0.283822945575014,0.378421775132442,
0.47302060468987,0.567619434247297,0.662231492256091,0.756843550264884,
0.851455608273677,0.94606766628247,1.0406664958399,1.13526532539733,1.22986415495475,
1.32446298451218,1.41907504252097,1.51368710052977),.UNSPECIFIED.);
#227=B_SPLINE_CURVE_WITH_KNOTS('',3,(#7092,#7093,#7094,#7095,#7096,#7097,
#7098,#7099,#7100,#7101,#7102,#7103,#7104,#7105,#7106,#7107,#7108,#7109,
#7110,#7111,#7112,#7113,#7114,#7115,#7116,#7117,#7118,#7119,#7120,#7121,
#7122,#7123,#7124,#7125),.UNSPECIFIED.,.T.,.F.,(4,2,2,2,2,2,2,2,2,2,2,2,
2,2,2,2,4),(0.,0.0946120580087934,0.189224116017587,0.283822945575014,0.378421775132442,
0.47302060468987,0.567619434247297,0.66223149225609,0.756843550264884,0.851455608273677,
0.94606766628247,1.0406664958399,1.13526532539733,1.22986415495475,1.32446298451218,
1.41907504252097,1.51368710052977),.UNSPECIFIED.);
#228=B_SPLINE_CURVE_WITH_KNOTS('',3,(#7129,#7130,#7131,#7132,#7133,#7134,
#7135,#7136,#7137,#7138),.UNSPECIFIED.,.F.,.F.,(4,2,2,2,4),(1.13193471301885,
1.22626174930539,1.32058878559194,1.41491753480854,1.50924628402513),
 .UNSPECIFIED.);
#229=B_SPLINE_CURVE_WITH_KNOTS('',3,(#7140,#7141,#7142,#7143,#7144,#7145,
#7146,#7147,#7148,#7149,#7150,#7151,#7152,#7153,#7154,#7155,#7156,#7157),
 .UNSPECIFIED.,.F.,.F.,(4,2,2,2,2,2,2,2,4),(0.377311571006283,0.47163860729283,
0.565965643579376,0.660294392795971,0.754623142012565,0.84895189122916,
0.943280640445755,1.0376076767323,1.13193471301885),.UNSPECIFIED.);
#230=B_SPLINE_CURVE_WITH_KNOTS('',3,(#7158,#7159,#7160,#7161,#7162,#7163,
#7164,#7165,#7166,#7167),.UNSPECIFIED.,.F.,.F.,(4,2,2,2,4),(1.50924628402513,
1.60357503324173,1.69790378245832,1.79223081874487,1.88655785503141),
 .UNSPECIFIED.);
#231=B_SPLINE_CURVE_WITH_KNOTS('',3,(#7176,#7177,#7178,#7179,#7180,#7181,
#7182,#7183,#7184,#7185,#7186,#7187,#7188,#7189,#7190,#7191,#7192,#7193),
 .UNSPECIFIED.,.F.,.F.,(4,2,2,2,2,2,2,2,4),(0.377311571006282,0.471638607292829,
0.565965643579376,0.660294392795971,0.754623142012565,0.84895189122916,
0.943280640445754,1.0376076767323,1.13193471301885),.UNSPECIFIED.);
#232=B_SPLINE_CURVE_WITH_KNOTS('',3,(#7195,#7196,#7197,#7198,#7199,#7200,
#7201,#7202,#7203,#7204),.UNSPECIFIED.,.F.,.F.,(4,2,2,2,4),(1.13193471301885,
1.22626174930539,1.32058878559194,1.41491753480854,1.50924628402513),
 .UNSPECIFIED.);
#233=B_SPLINE_CURVE_WITH_KNOTS('',3,(#7205,#7206,#7207,#7208,#7209,#7210,
#7211,#7212,#7213,#7214),.UNSPECIFIED.,.F.,.F.,(4,2,2,2,4),(1.50924628402513,
1.60357503324172,1.69790378245832,1.79223081874487,1.88655785503141),
 .UNSPECIFIED.);
#234=B_SPLINE_CURVE_WITH_KNOTS('',3,(#7217,#7218,#7219,#7220,#7221,#7222,
#7223,#7224,#7225,#7226,#7227,#7228,#7229,#7230,#7231,#7232,#7233,#7234),
 .UNSPECIFIED.,.F.,.F.,(4,2,2,2,2,2,2,2,4),(0.377311571006283,0.47163860729283,
0.565965643579376,0.660294392795971,0.754623142012565,0.84895189122916,
0.943280640445754,1.0376076767323,1.13193471301885),.UNSPECIFIED.);
#235=B_SPLINE_CURVE_WITH_KNOTS('',3,(#7236,#7237,#7238,#7239,#7240,#7241,
#7242,#7243,#7244,#7245),.UNSPECIFIED.,.F.,.F.,(4,2,2,2,4),(1.13193471301885,
1.22626174930539,1.32058878559194,1.41491753480854,1.50924628402513),
 .UNSPECIFIED.);
#236=B_SPLINE_CURVE_WITH_KNOTS('',3,(#7246,#7247,#7248,#7249,#7250,#7251,
#7252,#7253,#7254,#7255),.UNSPECIFIED.,.F.,.F.,(4,2,2,2,4),(1.50924628402513,
1.60357503324173,1.69790378245832,1.79223081874487,1.88655785503141),
 .UNSPECIFIED.);
#237=B_SPLINE_CURVE_WITH_KNOTS('',3,(#7258,#7259,#7260,#7261,#7262,#7263,
#7264,#7265,#7266,#7267,#7268,#7269,#7270,#7271,#7272,#7273,#7274,#7275),
 .UNSPECIFIED.,.F.,.F.,(4,2,2,2,2,2,2,2,4),(0.377311571006282,0.471638607292829,
0.565965643579376,0.66029439279597,0.754623142012565,0.84895189122916,0.943280640445754,
1.0376076767323,1.13193471301885),.UNSPECIFIED.);
#238=B_SPLINE_CURVE_WITH_KNOTS('',3,(#7277,#7278,#7279,#7280,#7281,#7282,
#7283,#7284,#7285,#7286),.UNSPECIFIED.,.F.,.F.,(4,2,2,2,4),(1.13193471301885,
1.22626174930539,1.32058878559194,1.41491753480854,1.50924628402513),
 .UNSPECIFIED.);
#239=B_SPLINE_CURVE_WITH_KNOTS('',3,(#7287,#7288,#7289,#7290,#7291,#7292,
#7293,#7294,#7295,#7296),.UNSPECIFIED.,.F.,.F.,(4,2,2,2,4),(1.50924628402513,
1.60357503324172,1.69790378245832,1.79223081874487,1.88655785503141),
 .UNSPECIFIED.);
#240=B_SPLINE_CURVE_WITH_KNOTS('',3,(#7299,#7300,#7301,#7302,#7303,#7304,
#7305,#7306,#7307,#7308,#7309,#7310,#7311,#7312,#7313,#7314,#7315,#7316),
 .UNSPECIFIED.,.F.,.F.,(4,2,2,2,2,2,2,2,4),(0.377311571006283,0.471638607292829,
0.565965643579376,0.660294392795971,0.754623142012565,0.84895189122916,
0.943280640445755,1.0376076767323,1.13193471301885),.UNSPECIFIED.);
#241=B_SPLINE_CURVE_WITH_KNOTS('',3,(#7318,#7319,#7320,#7321,#7322,#7323,
#7324,#7325,#7326,#7327),.UNSPECIFIED.,.F.,.F.,(4,2,2,2,4),(1.13193471301885,
1.22626174930539,1.32058878559194,1.41491753480854,1.50924628402513),
 .UNSPECIFIED.);
#242=B_SPLINE_CURVE_WITH_KNOTS('',3,(#7328,#7329,#7330,#7331,#7332,#7333,
#7334,#7335,#7336,#7337),.UNSPECIFIED.,.F.,.F.,(4,2,2,2,4),(1.50924628402513,
1.60357503324172,1.69790378245832,1.79223081874487,1.88655785503141),
 .UNSPECIFIED.);
#243=B_SPLINE_CURVE_WITH_KNOTS('',3,(#7341,#7342,#7343,#7344,#7345,#7346,
#7347,#7348,#7349,#7350,#7351,#7352,#7353,#7354,#7355,#7356,#7357,#7358,
#7359,#7360,#7361,#7362,#7363,#7364,#7365,#7366,#7367,#7368,#7369,#7370,
#7371,#7372,#7373,#7374),.UNSPECIFIED.,.T.,.F.,(4,2,2,2,2,2,2,2,2,2,2,2,
2,2,2,2,4),(0.,0.0946120580087934,0.189224116017587,0.283822945575014,0.378421775132442,
0.47302060468987,0.567619434247297,0.66223149225609,0.756843550264884,0.851455608273677,
0.94606766628247,1.0406664958399,1.13526532539733,1.22986415495475,1.32446298451218,
1.41907504252097,1.51368710052977),.UNSPECIFIED.);
#244=B_SPLINE_CURVE_WITH_KNOTS('',3,(#7377,#7378,#7379,#7380,#7381,#7382,
#7383,#7384,#7385,#7386,#7387,#7388,#7389,#7390,#7391,#7392,#7393,#7394,
#7395,#7396,#7397,#7398,#7399,#7400,#7401,#7402,#7403,#7404,#7405,#7406,
#7407,#7408,#7409,#7410),.UNSPECIFIED.,.T.,.F.,(4,2,2,2,2,2,2,2,2,2,2,2,
2,2,2,2,4),(0.,0.0946120580087934,0.189224116017587,0.283822945575014,0.378421775132442,
0.47302060468987,0.567619434247297,0.66223149225609,0.756843550264884,0.851455608273677,
0.94606766628247,1.0406664958399,1.13526532539733,1.22986415495475,1.32446298451218,
1.41907504252097,1.51368710052977),.UNSPECIFIED.);
#245=B_SPLINE_CURVE_WITH_KNOTS('',3,(#7415,#7416,#7417,#7418,#7419,#7420,
#7421,#7422,#7423,#7424,#7425,#7426,#7427,#7428,#7429,#7430,#7431,#7432,
#7433,#7434,#7435,#7436,#7437,#7438,#7439,#7440,#7441,#7442,#7443,#7444,
#7445,#7446,#7447,#7448),.UNSPECIFIED.,.T.,.F.,(4,2,2,2,2,2,2,2,2,2,2,2,
2,2,2,2,4),(0.,0.0946120580087934,0.189224116017587,0.283822945575014,0.378421775132442,
0.47302060468987,0.567619434247297,0.66223149225609,0.756843550264884,0.851455608273677,
0.94606766628247,1.0406664958399,1.13526532539733,1.22986415495475,1.32446298451218,
1.41907504252097,1.51368710052977),.UNSPECIFIED.);
#246=B_SPLINE_CURVE_WITH_KNOTS('',3,(#7451,#7452,#7453,#7454,#7455,#7456,
#7457,#7458,#7459,#7460,#7461,#7462,#7463,#7464,#7465,#7466,#7467,#7468,
#7469,#7470,#7471,#7472,#7473,#7474,#7475,#7476,#7477,#7478,#7479,#7480,
#7481,#7482,#7483,#7484),.UNSPECIFIED.,.T.,.F.,(4,2,2,2,2,2,2,2,2,2,2,2,
2,2,2,2,4),(0.,0.0946120580087934,0.189224116017587,0.283822945575014,0.378421775132442,
0.47302060468987,0.567619434247297,0.66223149225609,0.756843550264884,0.851455608273677,
0.94606766628247,1.0406664958399,1.13526532539733,1.22986415495475,1.32446298451218,
1.41907504252097,1.51368710052977),.UNSPECIFIED.);
#247=B_SPLINE_CURVE_WITH_KNOTS('',3,(#7700,#7701,#7702,#7703,#7704,#7705,
#7706,#7707,#7708,#7709),.UNSPECIFIED.,.F.,.F.,(4,2,2,2,4),(0.803821788694085,
0.87295099185362,0.952307212900969,1.03166343394832,1.10079263710785),
 .UNSPECIFIED.);
#248=B_SPLINE_CURVE_WITH_KNOTS('',3,(#7715,#7716,#7717,#7718,#7719,#7720,
#7721,#7722,#7723,#7724,#7725,#7726,#7727,#7728,#7729,#7730,#7731,#7732),
 .UNSPECIFIED.,.F.,.F.,(4,2,2,2,2,2,2,2,4),(0.,0.0791670250779307,0.158334050155861,
0.237500747381213,0.316667444606564,0.395834141831915,0.475000839057267,
0.554167864135197,0.633334889213128),.UNSPECIFIED.);
#249=B_SPLINE_CURVE_WITH_KNOTS('',3,(#7733,#7734,#7735,#7736,#7737,#7738,
#7739,#7740,#7741,#7742,#7743,#7744,#7745,#7746,#7747,#7748,#7749,#7750),
 .UNSPECIFIED.,.F.,.F.,(4,2,2,2,2,2,2,2,4),(0.633334889213128,0.712501914291059,
0.791668939368989,0.870835636594341,0.950002333819692,1.02916903104504,
1.10833572827039,1.18750275334833,1.26666977842626),.UNSPECIFIED.);
#250=B_SPLINE_CURVE_WITH_KNOTS('',3,(#7753,#7754,#7755,#7756,#7757,#7758,
#7759,#7760,#7761,#7762),.UNSPECIFIED.,.F.,.F.,(4,2,2,2,4),(0.168950313426771,
0.238079516586307,0.317435737633656,0.396791958681006,0.465921161840542),
 .UNSPECIFIED.);
#251=B_SPLINE_CURVE_WITH_KNOTS('',3,(#7805,#7806,#7807,#7808,#7809,#7810,
#7811,#7812,#7813,#7814),.UNSPECIFIED.,.F.,.F.,(4,2,2,2,4),(0.803821788694082,
0.872950991853617,0.952307212900967,1.03166343394832,1.10079263710785),
 .UNSPECIFIED.);
#252=B_SPLINE_CURVE_WITH_KNOTS('',3,(#7820,#7821,#7822,#7823,#7824,#7825,
#7826,#7827,#7828,#7829,#7830,#7831,#7832,#7833,#7834,#7835,#7836,#7837),
 .UNSPECIFIED.,.F.,.F.,(4,2,2,2,2,2,2,2,4),(0.,0.0791670250779298,0.15833405015586,
0.237500747381211,0.316667444606563,0.395834141831915,0.475000839057267,
0.554167864135197,0.633334889213127),.UNSPECIFIED.);
#253=B_SPLINE_CURVE_WITH_KNOTS('',3,(#7838,#7839,#7840,#7841,#7842,#7843,
#7844,#7845,#7846,#7847,#7848,#7849,#7850,#7851,#7852,#7853,#7854,#7855),
 .UNSPECIFIED.,.F.,.F.,(4,2,2,2,2,2,2,2,4),(0.633334889213127,0.712501914291057,
0.791668939368986,0.870835636594338,0.95000233381969,1.02916903104504,1.10833572827039,
1.18750275334832,1.26666977842625),.UNSPECIFIED.);
#254=B_SPLINE_CURVE_WITH_KNOTS('',3,(#7858,#7859,#7860,#7861,#7862,#7863,
#7864,#7865,#7866,#7867),.UNSPECIFIED.,.F.,.F.,(4,2,2,2,4),(0.168950313426766,
0.238079516586306,0.317435737633656,0.396791958681006,0.46592116184054),
 .UNSPECIFIED.);
#255=B_SPLINE_CURVE_WITH_KNOTS('',3,(#7910,#7911,#7912,#7913,#7914,#7915,
#7916,#7917,#7918,#7919,#7920,#7921,#7922,#7923),.UNSPECIFIED.,.F.,.F.,
(4,2,2,2,2,2,4),(0.75600573798702,0.793568827564647,0.872922520054201,0.952276212543756,
1.03162990503331,1.11098359752287,1.14854668710049),.UNSPECIFIED.);
#256=B_SPLINE_CURVE_WITH_KNOTS('',3,(#7929,#7930,#7931,#7932,#7933,#7934,
#7935,#7936,#7937,#7938,#7939,#7940,#7941,#7942,#7943,#7944,#7945,#7946),
 .UNSPECIFIED.,.F.,.F.,(4,2,2,2,2,2,2,2,4),(0.,0.079216580773363,0.158433161546726,
0.23764869707457,0.316864232602414,0.396079768130259,0.475295303658103,
0.554511884431466,0.633728465204829),.UNSPECIFIED.);
#257=B_SPLINE_CURVE_WITH_KNOTS('',3,(#7947,#7948,#7949,#7950,#7951,#7952,
#7953,#7954,#7955,#7956,#7957,#7958,#7959,#7960,#7961,#7962,#7963,#7964),
 .UNSPECIFIED.,.F.,.F.,(4,2,2,2,2,2,2,2,4),(0.633728465204829,0.712945045978192,
0.792161626751555,0.871377162279399,0.950592697807244,1.02980823333509,
1.10902376886293,1.18824034963629,1.26745693040966),.UNSPECIFIED.);
#258=B_SPLINE_CURVE_WITH_KNOTS('',3,(#7967,#7968,#7969,#7970,#7971,#7972,
#7973,#7974,#7975,#7976,#7977,#7978,#7979,#7980),.UNSPECIFIED.,.F.,.F.,
(4,2,2,2,2,2,4),(0.121154929624515,0.158718019202143,0.238071711691697,
0.317425404181252,0.396779096670807,0.476132789160362,0.513695878737989),
 .UNSPECIFIED.);
#259=B_SPLINE_CURVE_WITH_KNOTS('',3,(#8005,#8006,#8007,#8008,#8009,#8010,
#8011,#8012,#8013,#8014,#8015,#8016,#8017,#8018),.UNSPECIFIED.,.F.,.F.,
(4,2,2,2,2,2,4),(0.756005737987015,0.793568827564645,0.8729225200542,0.952276212543755,
1.03162990503331,1.11098359752287,1.1485466871005),.UNSPECIFIED.);
#260=B_SPLINE_CURVE_WITH_KNOTS('',3,(#8024,#8025,#8026,#8027,#8028,#8029,
#8030,#8031,#8032,#8033,#8034,#8035,#8036,#8037,#8038,#8039,#8040,#8041),
 .UNSPECIFIED.,.F.,.F.,(4,2,2,2,2,2,2,2,4),(0.,0.0792165807733624,0.158433161546725,
0.237648697074569,0.316864232602414,0.396079768130259,0.475295303658103,
0.554511884431466,0.633728465204828),.UNSPECIFIED.);
#261=B_SPLINE_CURVE_WITH_KNOTS('',3,(#8042,#8043,#8044,#8045,#8046,#8047,
#8048,#8049,#8050,#8051,#8052,#8053,#8054,#8055,#8056,#8057,#8058,#8059),
 .UNSPECIFIED.,.F.,.F.,(4,2,2,2,2,2,2,2,4),(0.633728465204828,0.712945045978191,
0.792161626751553,0.871377162279398,0.950592697807242,1.02980823333509,
1.10902376886293,1.18824034963629,1.26745693040966),.UNSPECIFIED.);
#262=B_SPLINE_CURVE_WITH_KNOTS('',3,(#8062,#8063,#8064,#8065,#8066,#8067,
#8068,#8069,#8070,#8071,#8072,#8073,#8074,#8075),.UNSPECIFIED.,.F.,.F.,
(4,2,2,2,2,2,4),(0.121154929624512,0.158718019202141,0.238071711691696,
0.317425404181252,0.396779096670807,0.476132789160362,0.513695878737992),
 .UNSPECIFIED.);
#263=SPHERICAL_SURFACE('',#4833,2.35);
#264=SPHERICAL_SURFACE('',#4873,2.35);
#265=ORIENTED_CLOSED_SHELL('',*,#4337,.F.);
#266=ORIENTED_CLOSED_SHELL('',*,#4342,.F.);
#267=ORIENTED_CLOSED_SHELL('',*,#4354,.F.);
#268=CONICAL_SURFACE('',#4802,0.475,0.785398163397449);
#269=CONICAL_SURFACE('',#4806,0.485,0.785398163397448);
#270=CONICAL_SURFACE('',#4810,0.31,0.463647609000806);
#271=CONICAL_SURFACE('',#4814,0.27,0.785398163397448);
#272=CONICAL_SURFACE('',#4919,0.625,0.785398163397448);
#273=CONICAL_SURFACE('',#4923,0.635,0.785398163397449);
#274=CONICAL_SURFACE('',#4927,0.41,0.463647609000806);
#275=CONICAL_SURFACE('',#5098,0.235,0.785398163397448);
#276=CONICAL_SURFACE('',#5102,0.2125,0.785398163397448);
#277=CONICAL_SURFACE('',#5108,0.4,0.785398163397448);
#278=CONICAL_SURFACE('',#5112,0.41,0.785398163397448);
#279=CONICAL_SURFACE('',#5116,0.26,0.463647609000806);
#280=CONICAL_SURFACE('',#5120,0.225,0.785398163397448);
#281=BREP_WITH_VOIDS('Body1',#4336,(#265));
#282=BREP_WITH_VOIDS('Body1',#4343,(#266));
#283=BREP_WITH_VOIDS('Body1',#4353,(#267));
#284=SHAPE_REPRESENTATION_RELATIONSHIP('SRR','None',#8499,#311);
#285=SHAPE_REPRESENTATION_RELATIONSHIP('SRR','None',#8500,#312);
#286=SHAPE_REPRESENTATION_RELATIONSHIP('SRR','None',#8501,#313);
#287=SHAPE_REPRESENTATION_RELATIONSHIP('SRR','None',#8502,#314);
#288=SHAPE_REPRESENTATION_RELATIONSHIP('SRR','None',#8503,#315);
#289=SHAPE_REPRESENTATION_RELATIONSHIP('SRR','None',#8504,#316);
#290=SHAPE_REPRESENTATION_RELATIONSHIP('SRR','None',#8505,#317);
#291=SHAPE_REPRESENTATION_RELATIONSHIP('SRR','None',#8506,#318);
#292=SHAPE_REPRESENTATION_RELATIONSHIP('SRR','None',#8507,#319);
#293=SHAPE_REPRESENTATION_RELATIONSHIP('SRR','None',#8508,#320);
#294=SHAPE_REPRESENTATION_RELATIONSHIP('SRR','None',#8509,#321);
#295=SHAPE_REPRESENTATION_RELATIONSHIP('SRR','None',#8510,#322);
#296=SHAPE_REPRESENTATION_RELATIONSHIP('SRR','None',#8511,#323);
#297=SHAPE_REPRESENTATION_RELATIONSHIP('SRR','None',#8513,#324);
#298=SHAPE_REPRESENTATION_RELATIONSHIP('SRR','None',#8514,#325);
#299=SHAPE_REPRESENTATION_RELATIONSHIP('SRR','None',#8515,#326);
#300=SHAPE_REPRESENTATION_RELATIONSHIP('SRR','None',#8516,#327);
#301=SHAPE_REPRESENTATION_RELATIONSHIP('SRR','None',#8518,#328);
#302=SHAPE_REPRESENTATION_RELATIONSHIP('SRR','None',#8519,#329);
#303=SHAPE_REPRESENTATION_RELATIONSHIP('SRR','None',#8520,#330);
#304=SHAPE_REPRESENTATION_RELATIONSHIP('SRR','None',#8521,#331);
#305=SHAPE_REPRESENTATION_RELATIONSHIP('SRR','None',#8522,#332);
#306=SHAPE_REPRESENTATION_RELATIONSHIP('SRR','None',#8523,#333);
#307=SHAPE_REPRESENTATION_RELATIONSHIP('SRR','None',#8524,#334);
#308=SHAPE_REPRESENTATION_RELATIONSHIP('SRR','None',#8525,#335);
#309=SHAPE_REPRESENTATION_RELATIONSHIP('SRR','None',#8526,#336);
#310=SHAPE_REPRESENTATION_RELATIONSHIP('SRR','None',#8527,#337);
#311=ADVANCED_BREP_SHAPE_REPRESENTATION('',(#366),#8348);
#312=ADVANCED_BREP_SHAPE_REPRESENTATION('',(#367),#8349);
#313=ADVANCED_BREP_SHAPE_REPRESENTATION('',(#368),#8350);
#314=ADVANCED_BREP_SHAPE_REPRESENTATION('',(#369),#8351);
#315=ADVANCED_BREP_SHAPE_REPRESENTATION('',(#370),#8352);
#316=ADVANCED_BREP_SHAPE_REPRESENTATION('',(#371),#8353);
#317=ADVANCED_BREP_SHAPE_REPRESENTATION('',(#372),#8354);
#318=ADVANCED_BREP_SHAPE_REPRESENTATION('',(#373),#8355);
#319=ADVANCED_BREP_SHAPE_REPRESENTATION('',(#374),#8356);
#320=ADVANCED_BREP_SHAPE_REPRESENTATION('',(#375),#8357);
#321=ADVANCED_BREP_SHAPE_REPRESENTATION('',(#376),#8358);
#322=ADVANCED_BREP_SHAPE_REPRESENTATION('',(#377),#8359);
#323=ADVANCED_BREP_SHAPE_REPRESENTATION('',(#281),#8360);
#324=ADVANCED_BREP_SHAPE_REPRESENTATION('',(#378),#8362);
#325=ADVANCED_BREP_SHAPE_REPRESENTATION('',(#379,#380),#8363);
#326=ADVANCED_BREP_SHAPE_REPRESENTATION('',(#381),#8364);
#327=ADVANCED_BREP_SHAPE_REPRESENTATION('',(#282),#8365);
#328=ADVANCED_BREP_SHAPE_REPRESENTATION('',(#382),#8367);
#329=ADVANCED_BREP_SHAPE_REPRESENTATION('',(#383),#8368);
#330=ADVANCED_BREP_SHAPE_REPRESENTATION('',(#384),#8369);
#331=ADVANCED_BREP_SHAPE_REPRESENTATION('',(#385),#8370);
#332=ADVANCED_BREP_SHAPE_REPRESENTATION('',(#386),#8371);
#333=ADVANCED_BREP_SHAPE_REPRESENTATION('',(#387),#8372);
#334=ADVANCED_BREP_SHAPE_REPRESENTATION('',(#388),#8373);
#335=ADVANCED_BREP_SHAPE_REPRESENTATION('',(#389),#8374);
#336=ADVANCED_BREP_SHAPE_REPRESENTATION('',(#390),#8375);
#337=ADVANCED_BREP_SHAPE_REPRESENTATION('',(#283),#8376);
#338=STYLED_ITEM('',(#8697),#366);
#339=STYLED_ITEM('',(#8732),#367);
#340=STYLED_ITEM('',(#8711),#368);
#341=STYLED_ITEM('',(#8732),#369);
#342=STYLED_ITEM('',(#8711),#370);
#343=STYLED_ITEM('',(#8732),#371);
#344=STYLED_ITEM('',(#8732),#372);
#345=STYLED_ITEM('',(#8732),#373);
#346=STYLED_ITEM('',(#8732),#374);
#347=STYLED_ITEM('',(#8732),#375);
#348=STYLED_ITEM('',(#8732),#376);
#349=STYLED_ITEM('',(#8725),#377);
#350=STYLED_ITEM('',(#8725),#281);
#351=STYLED_ITEM('',(#8697),#378);
#352=STYLED_ITEM('',(#8718),#379);
#353=STYLED_ITEM('',(#8718),#380);
#354=STYLED_ITEM('',(#8725),#381);
#355=STYLED_ITEM('',(#8725),#282);
#356=STYLED_ITEM('',(#8718),#382);
#357=STYLED_ITEM('',(#8704),#383);
#358=STYLED_ITEM('',(#8704),#384);
#359=STYLED_ITEM('',(#8704),#385);
#360=STYLED_ITEM('',(#8704),#386);
#361=STYLED_ITEM('',(#8718),#387);
#362=STYLED_ITEM('',(#8718),#388);
#363=STYLED_ITEM('',(#8718),#389);
#364=STYLED_ITEM('',(#8725),#390);
#365=STYLED_ITEM('',(#8725),#283);
#366=MANIFOLD_SOLID_BREP('Body1',#4324);
#367=MANIFOLD_SOLID_BREP('Body1',#4325);
#368=MANIFOLD_SOLID_BREP('Body1',#4326);
#369=MANIFOLD_SOLID_BREP('Body1',#4327);
#370=MANIFOLD_SOLID_BREP('Body1',#4328);
#371=MANIFOLD_SOLID_BREP('Body1',#4329);
#372=MANIFOLD_SOLID_BREP('Body1',#4330);
#373=MANIFOLD_SOLID_BREP('Body1',#4331);
#374=MANIFOLD_SOLID_BREP('Body1',#4332);
#375=MANIFOLD_SOLID_BREP('Body1',#4333);
#376=MANIFOLD_SOLID_BREP('Body1',#4334);
#377=MANIFOLD_SOLID_BREP('Body1',#4335);
#378=MANIFOLD_SOLID_BREP('Body1',#4338);
#379=MANIFOLD_SOLID_BREP('Body1',#4339);
#380=MANIFOLD_SOLID_BREP('Body2',#4340);
#381=MANIFOLD_SOLID_BREP('Body1',#4341);
#382=MANIFOLD_SOLID_BREP('Body1',#4344);
#383=MANIFOLD_SOLID_BREP('Body1',#4345);
#384=MANIFOLD_SOLID_BREP('Body1',#4346);
#385=MANIFOLD_SOLID_BREP('Body1',#4347);
#386=MANIFOLD_SOLID_BREP('Body1',#4348);
#387=MANIFOLD_SOLID_BREP('Body1',#4349);
#388=MANIFOLD_SOLID_BREP('Body1',#4350);
#389=MANIFOLD_SOLID_BREP('Body1',#4351);
#390=MANIFOLD_SOLID_BREP('Body1',#4352);
#391=FACE_BOUND('',#921,.T.);
#392=FACE_BOUND('',#922,.T.);
#393=FACE_BOUND('',#923,.T.);
#394=FACE_BOUND('',#924,.T.);
#395=FACE_BOUND('',#925,.T.);
#396=FACE_BOUND('',#926,.T.);
#397=FACE_BOUND('',#927,.T.);
#398=FACE_BOUND('',#928,.T.);
#399=FACE_BOUND('',#929,.T.);
#400=FACE_BOUND('',#930,.T.);
#401=FACE_BOUND('',#932,.T.);
#402=FACE_BOUND('',#933,.T.);
#403=FACE_BOUND('',#934,.T.);
#404=FACE_BOUND('',#935,.T.);
#405=FACE_BOUND('',#936,.T.);
#406=FACE_BOUND('',#937,.T.);
#407=FACE_BOUND('',#938,.T.);
#408=FACE_BOUND('',#939,.T.);
#409=FACE_BOUND('',#940,.T.);
#410=FACE_BOUND('',#941,.T.);
#411=FACE_BOUND('',#951,.T.);
#412=FACE_BOUND('',#952,.T.);
#413=FACE_BOUND('',#969,.T.);
#414=FACE_BOUND('',#970,.T.);
#415=FACE_BOUND('',#981,.T.);
#416=FACE_BOUND('',#983,.T.);
#417=FACE_BOUND('',#987,.T.);
#418=FACE_BOUND('',#989,.T.);
#419=FACE_BOUND('',#993,.T.);
#420=FACE_BOUND('',#995,.T.);
#421=FACE_BOUND('',#999,.T.);
#422=FACE_BOUND('',#1001,.T.);
#423=FACE_BOUND('',#1005,.T.);
#424=FACE_BOUND('',#1007,.T.);
#425=FACE_BOUND('',#1011,.T.);
#426=FACE_BOUND('',#1013,.T.);
#427=FACE_BOUND('',#1017,.T.);
#428=FACE_BOUND('',#1019,.T.);
#429=FACE_BOUND('',#1025,.T.);
#430=FACE_BOUND('',#1041,.T.);
#431=FACE_BOUND('',#1042,.T.);
#432=FACE_BOUND('',#1050,.T.);
#433=FACE_BOUND('',#1051,.T.);
#434=FACE_BOUND('',#1052,.T.);
#435=FACE_BOUND('',#1055,.T.);
#436=FACE_BOUND('',#1057,.T.);
#437=FACE_BOUND('',#1070,.T.);
#438=FACE_BOUND('',#1071,.T.);
#439=FACE_BOUND('',#1072,.T.);
#440=FACE_BOUND('',#1075,.T.);
#441=FACE_BOUND('',#1077,.T.);
#442=FACE_BOUND('',#1078,.T.);
#443=FACE_BOUND('',#1080,.T.);
#444=FACE_BOUND('',#1084,.T.);
#445=FACE_BOUND('',#1085,.T.);
#446=FACE_BOUND('',#1086,.T.);
#447=FACE_BOUND('',#1087,.T.);
#448=FACE_BOUND('',#1088,.T.);
#449=FACE_BOUND('',#1089,.T.);
#450=FACE_BOUND('',#1095,.T.);
#451=FACE_BOUND('',#1097,.T.);
#452=FACE_BOUND('',#1100,.T.);
#453=FACE_BOUND('',#1102,.T.);
#454=FACE_BOUND('',#1103,.T.);
#455=FACE_BOUND('',#1104,.T.);
#456=FACE_BOUND('',#1105,.T.);
#457=FACE_BOUND('',#1106,.T.);
#458=FACE_BOUND('',#1107,.T.);
#459=FACE_BOUND('',#1111,.T.);
#460=FACE_BOUND('',#1113,.T.);
#461=FACE_BOUND('',#1128,.T.);
#462=FACE_BOUND('',#1146,.T.);
#463=FACE_BOUND('',#1147,.T.);
#464=FACE_BOUND('',#1149,.T.);
#465=FACE_BOUND('',#1151,.T.);
#466=FACE_BOUND('',#1159,.T.);
#467=FACE_BOUND('',#1161,.T.);
#468=FACE_BOUND('',#1163,.T.);
#469=FACE_BOUND('',#1165,.T.);
#470=FACE_BOUND('',#1173,.T.);
#471=FACE_BOUND('',#1175,.T.);
#472=FACE_BOUND('',#1177,.T.);
#473=FACE_BOUND('',#1179,.T.);
#474=FACE_BOUND('',#1184,.T.);
#475=FACE_BOUND('',#1186,.T.);
#476=FACE_BOUND('',#1188,.T.);
#477=FACE_BOUND('',#1190,.T.);
#478=FACE_BOUND('',#1195,.T.);
#479=FACE_BOUND('',#1197,.T.);
#480=FACE_BOUND('',#1199,.T.);
#481=FACE_BOUND('',#1201,.T.);
#482=FACE_BOUND('',#1205,.T.);
#483=FACE_BOUND('',#1207,.T.);
#484=FACE_BOUND('',#1211,.T.);
#485=FACE_BOUND('',#1213,.T.);
#486=FACE_BOUND('',#1232,.T.);
#487=FACE_BOUND('',#1242,.T.);
#488=PLANE('',#4686);
#489=PLANE('',#4687);
#490=PLANE('',#4688);
#491=PLANE('',#4689);
#492=PLANE('',#4690);
#493=PLANE('',#4691);
#494=PLANE('',#4696);
#495=PLANE('',#4700);
#496=PLANE('',#4701);
#497=PLANE('',#4702);
#498=PLANE('',#4703);
#499=PLANE('',#4704);
#500=PLANE('',#4705);
#501=PLANE('',#4706);
#502=PLANE('',#4708);
#503=PLANE('',#4709);
#504=PLANE('',#4710);
#505=PLANE('',#4711);
#506=PLANE('',#4712);
#507=PLANE('',#4713);
#508=PLANE('',#4718);
#509=PLANE('',#4722);
#510=PLANE('',#4723);
#511=PLANE('',#4724);
#512=PLANE('',#4725);
#513=PLANE('',#4726);
#514=PLANE('',#4727);
#515=PLANE('',#4728);
#516=PLANE('',#4730);
#517=PLANE('',#4731);
#518=PLANE('',#4732);
#519=PLANE('',#4733);
#520=PLANE('',#4734);
#521=PLANE('',#4735);
#522=PLANE('',#4743);
#523=PLANE('',#4744);
#524=PLANE('',#4752);
#525=PLANE('',#4753);
#526=PLANE('',#4761);
#527=PLANE('',#4762);
#528=PLANE('',#4770);
#529=PLANE('',#4771);
#530=PLANE('',#4779);
#531=PLANE('',#4780);
#532=PLANE('',#4788);
#533=PLANE('',#4789);
#534=PLANE('',#4797);
#535=PLANE('',#4798);
#536=PLANE('',#4800);
#537=PLANE('',#4808);
#538=PLANE('',#4816);
#539=PLANE('',#4817);
#540=PLANE('',#4818);
#541=PLANE('',#4819);
#542=PLANE('',#4820);
#543=PLANE('',#4821);
#544=PLANE('',#4822);
#545=PLANE('',#4823);
#546=PLANE('',#4824);
#547=PLANE('',#4835);
#548=PLANE('',#4837);
#549=PLANE('',#4839);
#550=PLANE('',#4841);
#551=PLANE('',#4842);
#552=PLANE('',#4844);
#553=PLANE('',#4845);
#554=PLANE('',#4851);
#555=PLANE('',#4852);
#556=PLANE('',#4853);
#557=PLANE('',#4854);
#558=PLANE('',#4855);
#559=PLANE('',#4856);
#560=PLANE('',#4857);
#561=PLANE('',#4862);
#562=PLANE('',#4863);
#563=PLANE('',#4864);
#564=PLANE('',#4865);
#565=PLANE('',#4866);
#566=PLANE('',#4871);
#567=PLANE('',#4876);
#568=PLANE('',#4886);
#569=PLANE('',#4888);
#570=PLANE('',#4892);
#571=PLANE('',#4904);
#572=PLANE('',#4905);
#573=PLANE('',#4907);
#574=PLANE('',#4908);
#575=PLANE('',#4909);
#576=PLANE('',#4910);
#577=PLANE('',#4911);
#578=PLANE('',#4912);
#579=PLANE('',#4913);
#580=PLANE('',#4914);
#581=PLANE('',#4915);
#582=PLANE('',#4917);
#583=PLANE('',#4925);
#584=PLANE('',#4969);
#585=PLANE('',#4973);
#586=PLANE('',#4974);
#587=PLANE('',#4975);
#588=PLANE('',#4977);
#589=PLANE('',#4978);
#590=PLANE('',#4979);
#591=PLANE('',#4981);
#592=PLANE('',#4982);
#593=PLANE('',#4984);
#594=PLANE('',#4985);
#595=PLANE('',#4986);
#596=PLANE('',#4991);
#597=PLANE('',#4992);
#598=PLANE('',#4994);
#599=PLANE('',#4999);
#600=PLANE('',#5000);
#601=PLANE('',#5001);
#602=PLANE('',#5002);
#603=PLANE('',#5003);
#604=PLANE('',#5010);
#605=PLANE('',#5012);
#606=PLANE('',#5017);
#607=PLANE('',#5018);
#608=PLANE('',#5019);
#609=PLANE('',#5020);
#610=PLANE('',#5021);
#611=PLANE('',#5028);
#612=PLANE('',#5030);
#613=PLANE('',#5035);
#614=PLANE('',#5042);
#615=PLANE('',#5043);
#616=PLANE('',#5045);
#617=PLANE('',#5050);
#618=PLANE('',#5057);
#619=PLANE('',#5058);
#620=PLANE('',#5066);
#621=PLANE('',#5067);
#622=PLANE('',#5075);
#623=PLANE('',#5076);
#624=PLANE('',#5078);
#625=PLANE('',#5079);
#626=PLANE('',#5080);
#627=PLANE('',#5081);
#628=PLANE('',#5082);
#629=PLANE('',#5083);
#630=PLANE('',#5084);
#631=PLANE('',#5085);
#632=PLANE('',#5086);
#633=PLANE('',#5087);
#634=PLANE('',#5089);
#635=PLANE('',#5090);
#636=PLANE('',#5091);
#637=PLANE('',#5092);
#638=PLANE('',#5093);
#639=PLANE('',#5094);
#640=PLANE('',#5095);
#641=PLANE('',#5096);
#642=PLANE('',#5104);
#643=PLANE('',#5106);
#644=PLANE('',#5114);
#645=PLANE('',#5122);
#646=PLANE('',#5123);
#647=PLANE('',#5124);
#648=PLANE('',#5125);
#649=PLANE('',#5126);
#650=PLANE('',#5127);
#651=PLANE('',#5128);
#652=PLANE('',#5129);
#653=PLANE('',#5130);
#654=FACE_OUTER_BOUND('',#906,.T.);
#655=FACE_OUTER_BOUND('',#907,.T.);
#656=FACE_OUTER_BOUND('',#908,.T.);
#657=FACE_OUTER_BOUND('',#909,.T.);
#658=FACE_OUTER_BOUND('',#910,.T.);
#659=FACE_OUTER_BOUND('',#911,.T.);
#660=FACE_OUTER_BOUND('',#912,.T.);
#661=FACE_OUTER_BOUND('',#913,.T.);
#662=FACE_OUTER_BOUND('',#914,.T.);
#663=FACE_OUTER_BOUND('',#915,.T.);
#664=FACE_OUTER_BOUND('',#916,.T.);
#665=FACE_OUTER_BOUND('',#917,.T.);
#666=FACE_OUTER_BOUND('',#918,.T.);
#667=FACE_OUTER_BOUND('',#919,.T.);
#668=FACE_OUTER_BOUND('',#920,.T.);
#669=FACE_OUTER_BOUND('',#931,.T.);
#670=FACE_OUTER_BOUND('',#942,.T.);
#671=FACE_OUTER_BOUND('',#943,.T.);
#672=FACE_OUTER_BOUND('',#944,.T.);
#673=FACE_OUTER_BOUND('',#945,.T.);
#674=FACE_OUTER_BOUND('',#946,.T.);
#675=FACE_OUTER_BOUND('',#947,.T.);
#676=FACE_OUTER_BOUND('',#948,.T.);
#677=FACE_OUTER_BOUND('',#949,.T.);
#678=FACE_OUTER_BOUND('',#950,.T.);
#679=FACE_OUTER_BOUND('',#953,.T.);
#680=FACE_OUTER_BOUND('',#954,.T.);
#681=FACE_OUTER_BOUND('',#955,.T.);
#682=FACE_OUTER_BOUND('',#956,.T.);
#683=FACE_OUTER_BOUND('',#957,.T.);
#684=FACE_OUTER_BOUND('',#958,.T.);
#685=FACE_OUTER_BOUND('',#959,.T.);
#686=FACE_OUTER_BOUND('',#960,.T.);
#687=FACE_OUTER_BOUND('',#961,.T.);
#688=FACE_OUTER_BOUND('',#962,.T.);
#689=FACE_OUTER_BOUND('',#963,.T.);
#690=FACE_OUTER_BOUND('',#964,.T.);
#691=FACE_OUTER_BOUND('',#965,.T.);
#692=FACE_OUTER_BOUND('',#966,.T.);
#693=FACE_OUTER_BOUND('',#967,.T.);
#694=FACE_OUTER_BOUND('',#968,.T.);
#695=FACE_OUTER_BOUND('',#971,.T.);
#696=FACE_OUTER_BOUND('',#972,.T.);
#697=FACE_OUTER_BOUND('',#973,.T.);
#698=FACE_OUTER_BOUND('',#974,.T.);
#699=FACE_OUTER_BOUND('',#975,.T.);
#700=FACE_OUTER_BOUND('',#976,.T.);
#701=FACE_OUTER_BOUND('',#977,.T.);
#702=FACE_OUTER_BOUND('',#978,.T.);
#703=FACE_OUTER_BOUND('',#979,.T.);
#704=FACE_OUTER_BOUND('',#980,.T.);
#705=FACE_OUTER_BOUND('',#982,.T.);
#706=FACE_OUTER_BOUND('',#984,.T.);
#707=FACE_OUTER_BOUND('',#985,.T.);
#708=FACE_OUTER_BOUND('',#986,.T.);
#709=FACE_OUTER_BOUND('',#988,.T.);
#710=FACE_OUTER_BOUND('',#990,.T.);
#711=FACE_OUTER_BOUND('',#991,.T.);
#712=FACE_OUTER_BOUND('',#992,.T.);
#713=FACE_OUTER_BOUND('',#994,.T.);
#714=FACE_OUTER_BOUND('',#996,.T.);
#715=FACE_OUTER_BOUND('',#997,.T.);
#716=FACE_OUTER_BOUND('',#998,.T.);
#717=FACE_OUTER_BOUND('',#1000,.T.);
#718=FACE_OUTER_BOUND('',#1002,.T.);
#719=FACE_OUTER_BOUND('',#1003,.T.);
#720=FACE_OUTER_BOUND('',#1004,.T.);
#721=FACE_OUTER_BOUND('',#1006,.T.);
#722=FACE_OUTER_BOUND('',#1008,.T.);
#723=FACE_OUTER_BOUND('',#1009,.T.);
#724=FACE_OUTER_BOUND('',#1010,.T.);
#725=FACE_OUTER_BOUND('',#1012,.T.);
#726=FACE_OUTER_BOUND('',#1014,.T.);
#727=FACE_OUTER_BOUND('',#1015,.T.);
#728=FACE_OUTER_BOUND('',#1016,.T.);
#729=FACE_OUTER_BOUND('',#1018,.T.);
#730=FACE_OUTER_BOUND('',#1020,.T.);
#731=FACE_OUTER_BOUND('',#1021,.T.);
#732=FACE_OUTER_BOUND('',#1022,.T.);
#733=FACE_OUTER_BOUND('',#1023,.T.);
#734=FACE_OUTER_BOUND('',#1024,.T.);
#735=FACE_OUTER_BOUND('',#1026,.T.);
#736=FACE_OUTER_BOUND('',#1027,.T.);
#737=FACE_OUTER_BOUND('',#1028,.T.);
#738=FACE_OUTER_BOUND('',#1029,.T.);
#739=FACE_OUTER_BOUND('',#1030,.T.);
#740=FACE_OUTER_BOUND('',#1031,.T.);
#741=FACE_OUTER_BOUND('',#1032,.T.);
#742=FACE_OUTER_BOUND('',#1033,.T.);
#743=FACE_OUTER_BOUND('',#1034,.T.);
#744=FACE_OUTER_BOUND('',#1035,.T.);
#745=FACE_OUTER_BOUND('',#1036,.T.);
#746=FACE_OUTER_BOUND('',#1037,.T.);
#747=FACE_OUTER_BOUND('',#1038,.T.);
#748=FACE_OUTER_BOUND('',#1039,.T.);
#749=FACE_OUTER_BOUND('',#1040,.T.);
#750=FACE_OUTER_BOUND('',#1043,.T.);
#751=FACE_OUTER_BOUND('',#1044,.T.);
#752=FACE_OUTER_BOUND('',#1045,.T.);
#753=FACE_OUTER_BOUND('',#1046,.T.);
#754=FACE_OUTER_BOUND('',#1047,.T.);
#755=FACE_OUTER_BOUND('',#1048,.T.);
#756=FACE_OUTER_BOUND('',#1049,.T.);
#757=FACE_OUTER_BOUND('',#1053,.T.);
#758=FACE_OUTER_BOUND('',#1054,.T.);
#759=FACE_OUTER_BOUND('',#1056,.T.);
#760=FACE_OUTER_BOUND('',#1058,.T.);
#761=FACE_OUTER_BOUND('',#1059,.T.);
#762=FACE_OUTER_BOUND('',#1060,.T.);
#763=FACE_OUTER_BOUND('',#1061,.T.);
#764=FACE_OUTER_BOUND('',#1062,.T.);
#765=FACE_OUTER_BOUND('',#1063,.T.);
#766=FACE_OUTER_BOUND('',#1064,.T.);
#767=FACE_OUTER_BOUND('',#1065,.T.);
#768=FACE_OUTER_BOUND('',#1066,.T.);
#769=FACE_OUTER_BOUND('',#1067,.T.);
#770=FACE_OUTER_BOUND('',#1068,.T.);
#771=FACE_OUTER_BOUND('',#1069,.T.);
#772=FACE_OUTER_BOUND('',#1073,.T.);
#773=FACE_OUTER_BOUND('',#1074,.T.);
#774=FACE_OUTER_BOUND('',#1076,.T.);
#775=FACE_OUTER_BOUND('',#1079,.T.);
#776=FACE_OUTER_BOUND('',#1081,.T.);
#777=FACE_OUTER_BOUND('',#1082,.T.);
#778=FACE_OUTER_BOUND('',#1083,.T.);
#779=FACE_OUTER_BOUND('',#1090,.T.);
#780=FACE_OUTER_BOUND('',#1091,.T.);
#781=FACE_OUTER_BOUND('',#1092,.T.);
#782=FACE_OUTER_BOUND('',#1093,.T.);
#783=FACE_OUTER_BOUND('',#1094,.T.);
#784=FACE_OUTER_BOUND('',#1096,.T.);
#785=FACE_OUTER_BOUND('',#1098,.T.);
#786=FACE_OUTER_BOUND('',#1099,.T.);
#787=FACE_OUTER_BOUND('',#1101,.T.);
#788=FACE_OUTER_BOUND('',#1108,.T.);
#789=FACE_OUTER_BOUND('',#1109,.T.);
#790=FACE_OUTER_BOUND('',#1110,.T.);
#791=FACE_OUTER_BOUND('',#1112,.T.);
#792=FACE_OUTER_BOUND('',#1114,.T.);
#793=FACE_OUTER_BOUND('',#1115,.T.);
#794=FACE_OUTER_BOUND('',#1116,.T.);
#795=FACE_OUTER_BOUND('',#1117,.T.);
#796=FACE_OUTER_BOUND('',#1118,.T.);
#797=FACE_OUTER_BOUND('',#1119,.T.);
#798=FACE_OUTER_BOUND('',#1120,.T.);
#799=FACE_OUTER_BOUND('',#1121,.T.);
#800=FACE_OUTER_BOUND('',#1122,.T.);
#801=FACE_OUTER_BOUND('',#1123,.T.);
#802=FACE_OUTER_BOUND('',#1124,.T.);
#803=FACE_OUTER_BOUND('',#1125,.T.);
#804=FACE_OUTER_BOUND('',#1126,.T.);
#805=FACE_OUTER_BOUND('',#1127,.T.);
#806=FACE_OUTER_BOUND('',#1129,.T.);
#807=FACE_OUTER_BOUND('',#1130,.T.);
#808=FACE_OUTER_BOUND('',#1131,.T.);
#809=FACE_OUTER_BOUND('',#1132,.T.);
#810=FACE_OUTER_BOUND('',#1133,.T.);
#811=FACE_OUTER_BOUND('',#1134,.T.);
#812=FACE_OUTER_BOUND('',#1135,.T.);
#813=FACE_OUTER_BOUND('',#1136,.T.);
#814=FACE_OUTER_BOUND('',#1137,.T.);
#815=FACE_OUTER_BOUND('',#1138,.T.);
#816=FACE_OUTER_BOUND('',#1139,.T.);
#817=FACE_OUTER_BOUND('',#1140,.T.);
#818=FACE_OUTER_BOUND('',#1141,.T.);
#819=FACE_OUTER_BOUND('',#1142,.T.);
#820=FACE_OUTER_BOUND('',#1143,.T.);
#821=FACE_OUTER_BOUND('',#1144,.T.);
#822=FACE_OUTER_BOUND('',#1145,.T.);
#823=FACE_OUTER_BOUND('',#1148,.T.);
#824=FACE_OUTER_BOUND('',#1150,.T.);
#825=FACE_OUTER_BOUND('',#1152,.T.);
#826=FACE_OUTER_BOUND('',#1153,.T.);
#827=FACE_OUTER_BOUND('',#1154,.T.);
#828=FACE_OUTER_BOUND('',#1155,.T.);
#829=FACE_OUTER_BOUND('',#1156,.T.);
#830=FACE_OUTER_BOUND('',#1157,.T.);
#831=FACE_OUTER_BOUND('',#1158,.T.);
#832=FACE_OUTER_BOUND('',#1160,.T.);
#833=FACE_OUTER_BOUND('',#1162,.T.);
#834=FACE_OUTER_BOUND('',#1164,.T.);
#835=FACE_OUTER_BOUND('',#1166,.T.);
#836=FACE_OUTER_BOUND('',#1167,.T.);
#837=FACE_OUTER_BOUND('',#1168,.T.);
#838=FACE_OUTER_BOUND('',#1169,.T.);
#839=FACE_OUTER_BOUND('',#1170,.T.);
#840=FACE_OUTER_BOUND('',#1171,.T.);
#841=FACE_OUTER_BOUND('',#1172,.T.);
#842=FACE_OUTER_BOUND('',#1174,.T.);
#843=FACE_OUTER_BOUND('',#1176,.T.);
#844=FACE_OUTER_BOUND('',#1178,.T.);
#845=FACE_OUTER_BOUND('',#1180,.T.);
#846=FACE_OUTER_BOUND('',#1181,.T.);
#847=FACE_OUTER_BOUND('',#1182,.T.);
#848=FACE_OUTER_BOUND('',#1183,.T.);
#849=FACE_OUTER_BOUND('',#1185,.T.);
#850=FACE_OUTER_BOUND('',#1187,.T.);
#851=FACE_OUTER_BOUND('',#1189,.T.);
#852=FACE_OUTER_BOUND('',#1191,.T.);
#853=FACE_OUTER_BOUND('',#1192,.T.);
#854=FACE_OUTER_BOUND('',#1193,.T.);
#855=FACE_OUTER_BOUND('',#1194,.T.);
#856=FACE_OUTER_BOUND('',#1196,.T.);
#857=FACE_OUTER_BOUND('',#1198,.T.);
#858=FACE_OUTER_BOUND('',#1200,.T.);
#859=FACE_OUTER_BOUND('',#1202,.T.);
#860=FACE_OUTER_BOUND('',#1203,.T.);
#861=FACE_OUTER_BOUND('',#1204,.T.);
#862=FACE_OUTER_BOUND('',#1206,.T.);
#863=FACE_OUTER_BOUND('',#1208,.T.);
#864=FACE_OUTER_BOUND('',#1209,.T.);
#865=FACE_OUTER_BOUND('',#1210,.T.);
#866=FACE_OUTER_BOUND('',#1212,.T.);
#867=FACE_OUTER_BOUND('',#1214,.T.);
#868=FACE_OUTER_BOUND('',#1215,.T.);
#869=FACE_OUTER_BOUND('',#1216,.T.);
#870=FACE_OUTER_BOUND('',#1217,.T.);
#871=FACE_OUTER_BOUND('',#1218,.T.);
#872=FACE_OUTER_BOUND('',#1219,.T.);
#873=FACE_OUTER_BOUND('',#1220,.T.);
#874=FACE_OUTER_BOUND('',#1221,.T.);
#875=FACE_OUTER_BOUND('',#1222,.T.);
#876=FACE_OUTER_BOUND('',#1223,.T.);
#877=FACE_OUTER_BOUND('',#1224,.T.);
#878=FACE_OUTER_BOUND('',#1225,.T.);
#879=FACE_OUTER_BOUND('',#1226,.T.);
#880=FACE_OUTER_BOUND('',#1227,.T.);
#881=FACE_OUTER_BOUND('',#1228,.T.);
#882=FACE_OUTER_BOUND('',#1229,.T.);
#883=FACE_OUTER_BOUND('',#1230,.T.);
#884=FACE_OUTER_BOUND('',#1231,.T.);
#885=FACE_OUTER_BOUND('',#1233,.T.);
#886=FACE_OUTER_BOUND('',#1234,.T.);
#887=FACE_OUTER_BOUND('',#1235,.T.);
#888=FACE_OUTER_BOUND('',#1236,.T.);
#889=FACE_OUTER_BOUND('',#1237,.T.);
#890=FACE_OUTER_BOUND('',#1238,.T.);
#891=FACE_OUTER_BOUND('',#1239,.T.);
#892=FACE_OUTER_BOUND('',#1240,.T.);
#893=FACE_OUTER_BOUND('',#1241,.T.);
#894=FACE_OUTER_BOUND('',#1243,.T.);
#895=FACE_OUTER_BOUND('',#1244,.T.);
#896=FACE_OUTER_BOUND('',#1245,.T.);
#897=FACE_OUTER_BOUND('',#1246,.T.);
#898=FACE_OUTER_BOUND('',#1247,.T.);
#899=FACE_OUTER_BOUND('',#1248,.T.);
#900=FACE_OUTER_BOUND('',#1249,.T.);
#901=FACE_OUTER_BOUND('',#1250,.T.);
#902=FACE_OUTER_BOUND('',#1251,.T.);
#903=FACE_OUTER_BOUND('',#1252,.T.);
#904=FACE_OUTER_BOUND('',#1253,.T.);
#905=FACE_OUTER_BOUND('',#1254,.T.);
#906=EDGE_LOOP('',(#2949,#2950,#2951,#2952));
#907=EDGE_LOOP('',(#2953,#2954,#2955,#2956));
#908=EDGE_LOOP('',(#2957,#2958,#2959,#2960));
#909=EDGE_LOOP('',(#2961,#2962,#2963,#2964));
#910=EDGE_LOOP('',(#2965,#2966,#2967,#2968));
#911=EDGE_LOOP('',(#2969,#2970,#2971,#2972));
#912=EDGE_LOOP('',(#2973,#2974,#2975,#2976));
#913=EDGE_LOOP('',(#2977,#2978,#2979,#2980));
#914=EDGE_LOOP('',(#2981,#2982,#2983,#2984));
#915=EDGE_LOOP('',(#2985,#2986,#2987,#2988));
#916=EDGE_LOOP('',(#2989,#2990,#2991,#2992));
#917=EDGE_LOOP('',(#2993,#2994,#2995,#2996));
#918=EDGE_LOOP('',(#2997,#2998,#2999,#3000));
#919=EDGE_LOOP('',(#3001,#3002,#3003,#3004));
#920=EDGE_LOOP('',(#3005,#3006,#3007,#3008));
#921=EDGE_LOOP('',(#3009));
#922=EDGE_LOOP('',(#3010));
#923=EDGE_LOOP('',(#3011));
#924=EDGE_LOOP('',(#3012));
#925=EDGE_LOOP('',(#3013));
#926=EDGE_LOOP('',(#3014));
#927=EDGE_LOOP('',(#3015));
#928=EDGE_LOOP('',(#3016));
#929=EDGE_LOOP('',(#3017));
#930=EDGE_LOOP('',(#3018));
#931=EDGE_LOOP('',(#3019,#3020,#3021,#3022));
#932=EDGE_LOOP('',(#3023));
#933=EDGE_LOOP('',(#3024));
#934=EDGE_LOOP('',(#3025));
#935=EDGE_LOOP('',(#3026));
#936=EDGE_LOOP('',(#3027));
#937=EDGE_LOOP('',(#3028));
#938=EDGE_LOOP('',(#3029));
#939=EDGE_LOOP('',(#3030));
#940=EDGE_LOOP('',(#3031));
#941=EDGE_LOOP('',(#3032));
#942=EDGE_LOOP('',(#3033,#3034,#3035,#3036));
#943=EDGE_LOOP('',(#3037));
#944=EDGE_LOOP('',(#3038,#3039,#3040,#3041));
#945=EDGE_LOOP('',(#3042));
#946=EDGE_LOOP('',(#3043,#3044,#3045,#3046));
#947=EDGE_LOOP('',(#3047,#3048,#3049,#3050));
#948=EDGE_LOOP('',(#3051,#3052,#3053,#3054));
#949=EDGE_LOOP('',(#3055,#3056,#3057,#3058));
#950=EDGE_LOOP('',(#3059,#3060,#3061,#3062));
#951=EDGE_LOOP('',(#3063));
#952=EDGE_LOOP('',(#3064));
#953=EDGE_LOOP('',(#3065,#3066,#3067,#3068));
#954=EDGE_LOOP('',(#3069,#3070,#3071,#3072));
#955=EDGE_LOOP('',(#3073,#3074,#3075,#3076));
#956=EDGE_LOOP('',(#3077,#3078,#3079,#3080));
#957=EDGE_LOOP('',(#3081,#3082,#3083,#3084));
#958=EDGE_LOOP('',(#3085,#3086,#3087,#3088));
#959=EDGE_LOOP('',(#3089,#3090,#3091,#3092));
#960=EDGE_LOOP('',(#3093,#3094,#3095,#3096));
#961=EDGE_LOOP('',(#3097));
#962=EDGE_LOOP('',(#3098,#3099,#3100,#3101));
#963=EDGE_LOOP('',(#3102));
#964=EDGE_LOOP('',(#3103,#3104,#3105,#3106));
#965=EDGE_LOOP('',(#3107,#3108,#3109,#3110));
#966=EDGE_LOOP('',(#3111,#3112,#3113,#3114));
#967=EDGE_LOOP('',(#3115,#3116,#3117,#3118));
#968=EDGE_LOOP('',(#3119,#3120,#3121,#3122));
#969=EDGE_LOOP('',(#3123));
#970=EDGE_LOOP('',(#3124));
#971=EDGE_LOOP('',(#3125,#3126,#3127,#3128));
#972=EDGE_LOOP('',(#3129,#3130,#3131,#3132));
#973=EDGE_LOOP('',(#3133,#3134,#3135,#3136));
#974=EDGE_LOOP('',(#3137,#3138,#3139,#3140));
#975=EDGE_LOOP('',(#3141,#3142,#3143,#3144));
#976=EDGE_LOOP('',(#3145,#3146,#3147,#3148));
#977=EDGE_LOOP('',(#3149,#3150,#3151,#3152));
#978=EDGE_LOOP('',(#3153,#3154,#3155,#3156));
#979=EDGE_LOOP('',(#3157,#3158,#3159,#3160));
#980=EDGE_LOOP('',(#3161));
#981=EDGE_LOOP('',(#3162));
#982=EDGE_LOOP('',(#3163));
#983=EDGE_LOOP('',(#3164));
#984=EDGE_LOOP('',(#3165,#3166,#3167,#3168));
#985=EDGE_LOOP('',(#3169,#3170,#3171,#3172));
#986=EDGE_LOOP('',(#3173));
#987=EDGE_LOOP('',(#3174));
#988=EDGE_LOOP('',(#3175));
#989=EDGE_LOOP('',(#3176));
#990=EDGE_LOOP('',(#3177,#3178,#3179,#3180));
#991=EDGE_LOOP('',(#3181,#3182,#3183,#3184));
#992=EDGE_LOOP('',(#3185));
#993=EDGE_LOOP('',(#3186));
#994=EDGE_LOOP('',(#3187));
#995=EDGE_LOOP('',(#3188));
#996=EDGE_LOOP('',(#3189,#3190,#3191,#3192));
#997=EDGE_LOOP('',(#3193,#3194,#3195,#3196));
#998=EDGE_LOOP('',(#3197));
#999=EDGE_LOOP('',(#3198));
#1000=EDGE_LOOP('',(#3199));
#1001=EDGE_LOOP('',(#3200));
#1002=EDGE_LOOP('',(#3201,#3202,#3203,#3204));
#1003=EDGE_LOOP('',(#3205,#3206,#3207,#3208));
#1004=EDGE_LOOP('',(#3209));
#1005=EDGE_LOOP('',(#3210));
#1006=EDGE_LOOP('',(#3211));
#1007=EDGE_LOOP('',(#3212));
#1008=EDGE_LOOP('',(#3213,#3214,#3215,#3216));
#1009=EDGE_LOOP('',(#3217,#3218,#3219,#3220));
#1010=EDGE_LOOP('',(#3221));
#1011=EDGE_LOOP('',(#3222));
#1012=EDGE_LOOP('',(#3223));
#1013=EDGE_LOOP('',(#3224));
#1014=EDGE_LOOP('',(#3225,#3226,#3227,#3228));
#1015=EDGE_LOOP('',(#3229,#3230,#3231,#3232));
#1016=EDGE_LOOP('',(#3233));
#1017=EDGE_LOOP('',(#3234));
#1018=EDGE_LOOP('',(#3235));
#1019=EDGE_LOOP('',(#3236));
#1020=EDGE_LOOP('',(#3237));
#1021=EDGE_LOOP('',(#3238,#3239,#3240,#3241));
#1022=EDGE_LOOP('',(#3242,#3243,#3244,#3245));
#1023=EDGE_LOOP('',(#3246,#3247,#3248,#3249));
#1024=EDGE_LOOP('',(#3250));
#1025=EDGE_LOOP('',(#3251));
#1026=EDGE_LOOP('',(#3252,#3253,#3254,#3255));
#1027=EDGE_LOOP('',(#3256,#3257,#3258,#3259));
#1028=EDGE_LOOP('',(#3260,#3261,#3262,#3263));
#1029=EDGE_LOOP('',(#3264));
#1030=EDGE_LOOP('',(#3265,#3266,#3267,#3268));
#1031=EDGE_LOOP('',(#3269,#3270,#3271,#3272));
#1032=EDGE_LOOP('',(#3273,#3274,#3275,#3276));
#1033=EDGE_LOOP('',(#3277,#3278,#3279,#3280));
#1034=EDGE_LOOP('',(#3281,#3282,#3283,#3284));
#1035=EDGE_LOOP('',(#3285,#3286,#3287,#3288));
#1036=EDGE_LOOP('',(#3289,#3290,#3291,#3292,#3293,#3294));
#1037=EDGE_LOOP('',(#3295,#3296,#3297,#3298,#3299,#3300));
#1038=EDGE_LOOP('',(#3301,#3302,#3303,#3304));
#1039=EDGE_LOOP('',(#3305,#3306,#3307,#3308));
#1040=EDGE_LOOP('',(#3309,#3310));
#1041=EDGE_LOOP('',(#3311));
#1042=EDGE_LOOP('',(#3312));
#1043=EDGE_LOOP('',(#3313,#3314,#3315));
#1044=EDGE_LOOP('',(#3316,#3317,#3318));
#1045=EDGE_LOOP('',(#3319,#3320,#3321));
#1046=EDGE_LOOP('',(#3322,#3323,#3324,#3325));
#1047=EDGE_LOOP('',(#3326,#3327,#3328));
#1048=EDGE_LOOP('',(#3329,#3330,#3331,#3332));
#1049=EDGE_LOOP('',(#3333,#3334,#3335,#3336));
#1050=EDGE_LOOP('',(#3337));
#1051=EDGE_LOOP('',(#3338));
#1052=EDGE_LOOP('',(#3339,#3340,#3341,#3342,#3343,#3344,#3345,#3346,#3347,
#3348,#3349,#3350));
#1053=EDGE_LOOP('',(#3351,#3352,#3353,#3354,#3355,#3356,#3357,#3358,#3359,
#3360,#3361,#3362));
#1054=EDGE_LOOP('',(#3363,#3364));
#1055=EDGE_LOOP('',(#3365));
#1056=EDGE_LOOP('',(#3366,#3367));
#1057=EDGE_LOOP('',(#3368));
#1058=EDGE_LOOP('',(#3369,#3370,#3371,#3372));
#1059=EDGE_LOOP('',(#3373,#3374,#3375,#3376));
#1060=EDGE_LOOP('',(#3377,#3378,#3379,#3380));
#1061=EDGE_LOOP('',(#3381,#3382,#3383,#3384));
#1062=EDGE_LOOP('',(#3385,#3386,#3387,#3388));
#1063=EDGE_LOOP('',(#3389,#3390,#3391,#3392));
#1064=EDGE_LOOP('',(#3393,#3394,#3395,#3396));
#1065=EDGE_LOOP('',(#3397,#3398,#3399,#3400));
#1066=EDGE_LOOP('',(#3401,#3402,#3403,#3404));
#1067=EDGE_LOOP('',(#3405,#3406,#3407,#3408));
#1068=EDGE_LOOP('',(#3409,#3410,#3411,#3412));
#1069=EDGE_LOOP('',(#3413,#3414,#3415,#3416));
#1070=EDGE_LOOP('',(#3417,#3418,#3419,#3420));
#1071=EDGE_LOOP('',(#3421));
#1072=EDGE_LOOP('',(#3422));
#1073=EDGE_LOOP('',(#3423,#3424,#3425,#3426));
#1074=EDGE_LOOP('',(#3427));
#1075=EDGE_LOOP('',(#3428));
#1076=EDGE_LOOP('',(#3429,#3430));
#1077=EDGE_LOOP('',(#3431));
#1078=EDGE_LOOP('',(#3432));
#1079=EDGE_LOOP('',(#3433));
#1080=EDGE_LOOP('',(#3434));
#1081=EDGE_LOOP('',(#3435,#3436,#3437,#3438,#3439,#3440));
#1082=EDGE_LOOP('',(#3441,#3442,#3443,#3444,#3445,#3446));
#1083=EDGE_LOOP('',(#3447,#3448,#3449,#3450));
#1084=EDGE_LOOP('',(#3451,#3452,#3453));
#1085=EDGE_LOOP('',(#3454,#3455,#3456));
#1086=EDGE_LOOP('',(#3457,#3458,#3459));
#1087=EDGE_LOOP('',(#3460,#3461,#3462));
#1088=EDGE_LOOP('',(#3463,#3464,#3465));
#1089=EDGE_LOOP('',(#3466,#3467,#3468));
#1090=EDGE_LOOP('',(#3469,#3470,#3471,#3472,#3473,#3474));
#1091=EDGE_LOOP('',(#3475,#3476,#3477,#3478,#3479,#3480));
#1092=EDGE_LOOP('',(#3481,#3482,#3483,#3484,#3485,#3486));
#1093=EDGE_LOOP('',(#3487,#3488,#3489,#3490,#3491,#3492));
#1094=EDGE_LOOP('',(#3493));
#1095=EDGE_LOOP('',(#3494));
#1096=EDGE_LOOP('',(#3495));
#1097=EDGE_LOOP('',(#3496));
#1098=EDGE_LOOP('',(#3497,#3498,#3499,#3500));
#1099=EDGE_LOOP('',(#3501));
#1100=EDGE_LOOP('',(#3502));
#1101=EDGE_LOOP('',(#3503,#3504,#3505,#3506));
#1102=EDGE_LOOP('',(#3507));
#1103=EDGE_LOOP('',(#3508));
#1104=EDGE_LOOP('',(#3509));
#1105=EDGE_LOOP('',(#3510));
#1106=EDGE_LOOP('',(#3511));
#1107=EDGE_LOOP('',(#3512));
#1108=EDGE_LOOP('',(#3513,#3514,#3515,#3516));
#1109=EDGE_LOOP('',(#3517,#3518,#3519,#3520));
#1110=EDGE_LOOP('',(#3521));
#1111=EDGE_LOOP('',(#3522));
#1112=EDGE_LOOP('',(#3523));
#1113=EDGE_LOOP('',(#3524));
#1114=EDGE_LOOP('',(#3525,#3526,#3527,#3528));
#1115=EDGE_LOOP('',(#3529,#3530,#3531,#3532));
#1116=EDGE_LOOP('',(#3533,#3534,#3535,#3536));
#1117=EDGE_LOOP('',(#3537,#3538,#3539,#3540));
#1118=EDGE_LOOP('',(#3541,#3542,#3543,#3544));
#1119=EDGE_LOOP('',(#3545,#3546,#3547,#3548));
#1120=EDGE_LOOP('',(#3549,#3550,#3551,#3552,#3553,#3554));
#1121=EDGE_LOOP('',(#3555,#3556,#3557,#3558,#3559,#3560));
#1122=EDGE_LOOP('',(#3561));
#1123=EDGE_LOOP('',(#3562));
#1124=EDGE_LOOP('',(#3563,#3564,#3565,#3566));
#1125=EDGE_LOOP('',(#3567,#3568,#3569,#3570));
#1126=EDGE_LOOP('',(#3571,#3572,#3573,#3574));
#1127=EDGE_LOOP('',(#3575));
#1128=EDGE_LOOP('',(#3576));
#1129=EDGE_LOOP('',(#3577,#3578,#3579,#3580));
#1130=EDGE_LOOP('',(#3581,#3582,#3583,#3584));
#1131=EDGE_LOOP('',(#3585,#3586,#3587,#3588));
#1132=EDGE_LOOP('',(#3589));
#1133=EDGE_LOOP('',(#3590,#3591,#3592,#3593));
#1134=EDGE_LOOP('',(#3594));
#1135=EDGE_LOOP('',(#3595,#3596,#3597,#3598));
#1136=EDGE_LOOP('',(#3599,#3600,#3601,#3602));
#1137=EDGE_LOOP('',(#3603,#3604,#3605,#3606));
#1138=EDGE_LOOP('',(#3607,#3608,#3609,#3610));
#1139=EDGE_LOOP('',(#3611,#3612,#3613,#3614));
#1140=EDGE_LOOP('',(#3615,#3616,#3617,#3618));
#1141=EDGE_LOOP('',(#3619,#3620,#3621,#3622));
#1142=EDGE_LOOP('',(#3623,#3624,#3625,#3626));
#1143=EDGE_LOOP('',(#3627,#3628,#3629,#3630));
#1144=EDGE_LOOP('',(#3631,#3632,#3633,#3634));
#1145=EDGE_LOOP('',(#3635,#3636,#3637,#3638));
#1146=EDGE_LOOP('',(#3639,#3640,#3641,#3642));
#1147=EDGE_LOOP('',(#3643,#3644,#3645,#3646));
#1148=EDGE_LOOP('',(#3647));
#1149=EDGE_LOOP('',(#3648));
#1150=EDGE_LOOP('',(#3649));
#1151=EDGE_LOOP('',(#3650));
#1152=EDGE_LOOP('',(#3651,#3652));
#1153=EDGE_LOOP('',(#3653,#3654,#3655,#3656,#3657,#3658,#3659,#3660,#3661));
#1154=EDGE_LOOP('',(#3662,#3663,#3664));
#1155=EDGE_LOOP('',(#3665,#3666,#3667,#3668));
#1156=EDGE_LOOP('',(#3669,#3670,#3671,#3672));
#1157=EDGE_LOOP('',(#3673,#3674,#3675,#3676));
#1158=EDGE_LOOP('',(#3677));
#1159=EDGE_LOOP('',(#3678,#3679,#3680,#3681));
#1160=EDGE_LOOP('',(#3682,#3683,#3684,#3685));
#1161=EDGE_LOOP('',(#3686,#3687,#3688,#3689));
#1162=EDGE_LOOP('',(#3690,#3691,#3692,#3693));
#1163=EDGE_LOOP('',(#3694,#3695));
#1164=EDGE_LOOP('',(#3696));
#1165=EDGE_LOOP('',(#3697,#3698,#3699,#3700));
#1166=EDGE_LOOP('',(#3701,#3702));
#1167=EDGE_LOOP('',(#3703,#3704,#3705,#3706,#3707,#3708,#3709,#3710,#3711));
#1168=EDGE_LOOP('',(#3712,#3713,#3714));
#1169=EDGE_LOOP('',(#3715,#3716,#3717,#3718));
#1170=EDGE_LOOP('',(#3719,#3720,#3721,#3722));
#1171=EDGE_LOOP('',(#3723,#3724,#3725,#3726));
#1172=EDGE_LOOP('',(#3727));
#1173=EDGE_LOOP('',(#3728,#3729,#3730,#3731));
#1174=EDGE_LOOP('',(#3732,#3733,#3734,#3735));
#1175=EDGE_LOOP('',(#3736,#3737,#3738,#3739));
#1176=EDGE_LOOP('',(#3740,#3741,#3742,#3743));
#1177=EDGE_LOOP('',(#3744,#3745));
#1178=EDGE_LOOP('',(#3746));
#1179=EDGE_LOOP('',(#3747,#3748,#3749,#3750));
#1180=EDGE_LOOP('',(#3751,#3752));
#1181=EDGE_LOOP('',(#3753,#3754,#3755,#3756,#3757,#3758,#3759,#3760,#3761));
#1182=EDGE_LOOP('',(#3762,#3763,#3764));
#1183=EDGE_LOOP('',(#3765,#3766,#3767,#3768));
#1184=EDGE_LOOP('',(#3769,#3770,#3771,#3772));
#1185=EDGE_LOOP('',(#3773,#3774,#3775,#3776));
#1186=EDGE_LOOP('',(#3777,#3778));
#1187=EDGE_LOOP('',(#3779));
#1188=EDGE_LOOP('',(#3780));
#1189=EDGE_LOOP('',(#3781));
#1190=EDGE_LOOP('',(#3782));
#1191=EDGE_LOOP('',(#3783,#3784));
#1192=EDGE_LOOP('',(#3785,#3786,#3787,#3788,#3789,#3790,#3791,#3792,#3793));
#1193=EDGE_LOOP('',(#3794,#3795,#3796));
#1194=EDGE_LOOP('',(#3797,#3798,#3799,#3800));
#1195=EDGE_LOOP('',(#3801,#3802,#3803,#3804));
#1196=EDGE_LOOP('',(#3805,#3806,#3807,#3808));
#1197=EDGE_LOOP('',(#3809,#3810));
#1198=EDGE_LOOP('',(#3811));
#1199=EDGE_LOOP('',(#3812));
#1200=EDGE_LOOP('',(#3813));
#1201=EDGE_LOOP('',(#3814));
#1202=EDGE_LOOP('',(#3815,#3816,#3817,#3818));
#1203=EDGE_LOOP('',(#3819,#3820,#3821,#3822));
#1204=EDGE_LOOP('',(#3823));
#1205=EDGE_LOOP('',(#3824));
#1206=EDGE_LOOP('',(#3825));
#1207=EDGE_LOOP('',(#3826));
#1208=EDGE_LOOP('',(#3827,#3828,#3829,#3830));
#1209=EDGE_LOOP('',(#3831,#3832,#3833,#3834));
#1210=EDGE_LOOP('',(#3835));
#1211=EDGE_LOOP('',(#3836));
#1212=EDGE_LOOP('',(#3837));
#1213=EDGE_LOOP('',(#3838));
#1214=EDGE_LOOP('',(#3839,#3840,#3841,#3842,#3843,#3844,#3845,#3846));
#1215=EDGE_LOOP('',(#3847,#3848,#3849,#3850));
#1216=EDGE_LOOP('',(#3851,#3852,#3853,#3854));
#1217=EDGE_LOOP('',(#3855,#3856,#3857,#3858));
#1218=EDGE_LOOP('',(#3859,#3860,#3861,#3862));
#1219=EDGE_LOOP('',(#3863,#3864,#3865,#3866,#3867,#3868,#3869,#3870));
#1220=EDGE_LOOP('',(#3871,#3872,#3873,#3874));
#1221=EDGE_LOOP('',(#3875,#3876,#3877,#3878));
#1222=EDGE_LOOP('',(#3879,#3880,#3881,#3882));
#1223=EDGE_LOOP('',(#3883,#3884,#3885,#3886));
#1224=EDGE_LOOP('',(#3887,#3888,#3889,#3890));
#1225=EDGE_LOOP('',(#3891,#3892,#3893,#3894));
#1226=EDGE_LOOP('',(#3895,#3896,#3897,#3898));
#1227=EDGE_LOOP('',(#3899,#3900,#3901,#3902));
#1228=EDGE_LOOP('',(#3903,#3904,#3905,#3906));
#1229=EDGE_LOOP('',(#3907,#3908,#3909,#3910));
#1230=EDGE_LOOP('',(#3911,#3912,#3913,#3914,#3915,#3916));
#1231=EDGE_LOOP('',(#3917));
#1232=EDGE_LOOP('',(#3918,#3919,#3920,#3921,#3922,#3923));
#1233=EDGE_LOOP('',(#3924,#3925,#3926,#3927));
#1234=EDGE_LOOP('',(#3928,#3929,#3930,#3931));
#1235=EDGE_LOOP('',(#3932,#3933,#3934,#3935));
#1236=EDGE_LOOP('',(#3936));
#1237=EDGE_LOOP('',(#3937));
#1238=EDGE_LOOP('',(#3938,#3939,#3940,#3941));
#1239=EDGE_LOOP('',(#3942,#3943,#3944,#3945));
#1240=EDGE_LOOP('',(#3946,#3947,#3948,#3949));
#1241=EDGE_LOOP('',(#3950));
#1242=EDGE_LOOP('',(#3951));
#1243=EDGE_LOOP('',(#3952,#3953,#3954,#3955));
#1244=EDGE_LOOP('',(#3956,#3957,#3958,#3959));
#1245=EDGE_LOOP('',(#3960,#3961,#3962,#3963));
#1246=EDGE_LOOP('',(#3964));
#1247=EDGE_LOOP('',(#3965,#3966,#3967,#3968));
#1248=EDGE_LOOP('',(#3969,#3970,#3971,#3972));
#1249=EDGE_LOOP('',(#3973,#3974,#3975,#3976));
#1250=EDGE_LOOP('',(#3977,#3978,#3979,#3980));
#1251=EDGE_LOOP('',(#3981,#3982,#3983,#3984));
#1252=EDGE_LOOP('',(#3985,#3986,#3987,#3988));
#1253=EDGE_LOOP('',(#3989,#3990,#3991,#3992,#3993,#3994));
#1254=EDGE_LOOP('',(#3995,#3996,#3997,#3998,#3999,#4000));
#1255=LINE('',#6472,#1582);
#1256=LINE('',#6478,#1583);
#1257=LINE('',#6484,#1584);
#1258=LINE('',#6490,#1585);
#1259=LINE('',#6496,#1586);
#1260=LINE('',#6502,#1587);
#1261=LINE('',#6508,#1588);
#1262=LINE('',#6514,#1589);
#1263=LINE('',#6520,#1590);
#1264=LINE('',#6526,#1591);
#1265=LINE('',#6531,#1592);
#1266=LINE('',#6533,#1593);
#1267=LINE('',#6535,#1594);
#1268=LINE('',#6536,#1595);
#1269=LINE('',#6539,#1596);
#1270=LINE('',#6541,#1597);
#1271=LINE('',#6542,#1598);
#1272=LINE('',#6545,#1599);
#1273=LINE('',#6547,#1600);
#1274=LINE('',#6548,#1601);
#1275=LINE('',#6550,#1602);
#1276=LINE('',#6551,#1603);
#1277=LINE('',#6559,#1604);
#1278=LINE('',#6566,#1605);
#1279=LINE('',#6572,#1606);
#1280=LINE('',#6574,#1607);
#1281=LINE('',#6576,#1608);
#1282=LINE('',#6577,#1609);
#1283=LINE('',#6580,#1610);
#1284=LINE('',#6582,#1611);
#1285=LINE('',#6583,#1612);
#1286=LINE('',#6586,#1613);
#1287=LINE('',#6588,#1614);
#1288=LINE('',#6589,#1615);
#1289=LINE('',#6591,#1616);
#1290=LINE('',#6592,#1617);
#1291=LINE('',#6599,#1618);
#1292=LINE('',#6601,#1619);
#1293=LINE('',#6603,#1620);
#1294=LINE('',#6604,#1621);
#1295=LINE('',#6607,#1622);
#1296=LINE('',#6609,#1623);
#1297=LINE('',#6610,#1624);
#1298=LINE('',#6613,#1625);
#1299=LINE('',#6615,#1626);
#1300=LINE('',#6616,#1627);
#1301=LINE('',#6618,#1628);
#1302=LINE('',#6619,#1629);
#1303=LINE('',#6627,#1630);
#1304=LINE('',#6634,#1631);
#1305=LINE('',#6640,#1632);
#1306=LINE('',#6642,#1633);
#1307=LINE('',#6644,#1634);
#1308=LINE('',#6645,#1635);
#1309=LINE('',#6648,#1636);
#1310=LINE('',#6650,#1637);
#1311=LINE('',#6651,#1638);
#1312=LINE('',#6654,#1639);
#1313=LINE('',#6656,#1640);
#1314=LINE('',#6657,#1641);
#1315=LINE('',#6659,#1642);
#1316=LINE('',#6660,#1643);
#1317=LINE('',#6667,#1644);
#1318=LINE('',#6669,#1645);
#1319=LINE('',#6671,#1646);
#1320=LINE('',#6672,#1647);
#1321=LINE('',#6675,#1648);
#1322=LINE('',#6677,#1649);
#1323=LINE('',#6678,#1650);
#1324=LINE('',#6681,#1651);
#1325=LINE('',#6683,#1652);
#1326=LINE('',#6684,#1653);
#1327=LINE('',#6686,#1654);
#1328=LINE('',#6687,#1655);
#1329=LINE('',#6695,#1656);
#1330=LINE('',#6701,#1657);
#1331=LINE('',#6710,#1658);
#1332=LINE('',#6716,#1659);
#1333=LINE('',#6725,#1660);
#1334=LINE('',#6731,#1661);
#1335=LINE('',#6740,#1662);
#1336=LINE('',#6746,#1663);
#1337=LINE('',#6755,#1664);
#1338=LINE('',#6761,#1665);
#1339=LINE('',#6770,#1666);
#1340=LINE('',#6776,#1667);
#1341=LINE('',#6785,#1668);
#1342=LINE('',#6791,#1669);
#1343=LINE('',#6802,#1670);
#1344=LINE('',#6806,#1671);
#1345=LINE('',#6810,#1672);
#1346=LINE('',#6817,#1673);
#1347=LINE('',#6821,#1674);
#1348=LINE('',#6825,#1675);
#1349=LINE('',#6830,#1676);
#1350=LINE('',#6832,#1677);
#1351=LINE('',#6834,#1678);
#1352=LINE('',#6835,#1679);
#1353=LINE('',#6838,#1680);
#1354=LINE('',#6840,#1681);
#1355=LINE('',#6841,#1682);
#1356=LINE('',#6844,#1683);
#1357=LINE('',#6846,#1684);
#1358=LINE('',#6847,#1685);
#1359=LINE('',#6850,#1686);
#1360=LINE('',#6852,#1687);
#1361=LINE('',#6853,#1688);
#1362=LINE('',#6856,#1689);
#1363=LINE('',#6858,#1690);
#1364=LINE('',#6859,#1691);
#1365=LINE('',#6861,#1692);
#1366=LINE('',#6862,#1693);
#1367=LINE('',#6871,#1694);
#1368=LINE('',#6877,#1695);
#1369=LINE('',#6886,#1696);
#1370=LINE('',#6888,#1697);
#1371=LINE('',#6893,#1698);
#1372=LINE('',#6896,#1699);
#1373=LINE('',#6900,#1700);
#1374=LINE('',#6903,#1701);
#1375=LINE('',#6905,#1702);
#1376=LINE('',#6906,#1703);
#1377=LINE('',#6910,#1704);
#1378=LINE('',#6912,#1705);
#1379=LINE('',#6915,#1706);
#1380=LINE('',#6916,#1707);
#1381=LINE('',#6920,#1708);
#1382=LINE('',#6922,#1709);
#1383=LINE('',#6924,#1710);
#1384=LINE('',#6925,#1711);
#1385=LINE('',#6931,#1712);
#1386=LINE('',#6933,#1713);
#1387=LINE('',#6934,#1714);
#1388=LINE('',#6936,#1715);
#1389=LINE('',#6938,#1716);
#1390=LINE('',#6939,#1717);
#1391=LINE('',#6948,#1718);
#1392=LINE('',#6950,#1719);
#1393=LINE('',#6952,#1720);
#1394=LINE('',#6953,#1721);
#1395=LINE('',#6956,#1722);
#1396=LINE('',#6958,#1723);
#1397=LINE('',#6959,#1724);
#1398=LINE('',#6962,#1725);
#1399=LINE('',#6964,#1726);
#1400=LINE('',#6965,#1727);
#1401=LINE('',#6967,#1728);
#1402=LINE('',#6968,#1729);
#1403=LINE('',#6973,#1730);
#1404=LINE('',#6977,#1731);
#1405=LINE('',#6981,#1732);
#1406=LINE('',#6982,#1733);
#1407=LINE('',#6983,#1734);
#1408=LINE('',#6986,#1735);
#1409=LINE('',#6987,#1736);
#1410=LINE('',#6990,#1737);
#1411=LINE('',#6991,#1738);
#1412=LINE('',#6993,#1739);
#1413=LINE('',#7000,#1740);
#1414=LINE('',#7055,#1741);
#1415=LINE('',#7127,#1742);
#1416=LINE('',#7172,#1743);
#1417=LINE('',#7340,#1744);
#1418=LINE('',#7411,#1745);
#1419=LINE('',#7414,#1746);
#1420=LINE('',#7485,#1747);
#1421=LINE('',#7495,#1748);
#1422=LINE('',#7500,#1749);
#1423=LINE('',#7508,#1750);
#1424=LINE('',#7514,#1751);
#1425=LINE('',#7522,#1752);
#1426=LINE('',#7524,#1753);
#1427=LINE('',#7526,#1754);
#1428=LINE('',#7527,#1755);
#1429=LINE('',#7530,#1756);
#1430=LINE('',#7532,#1757);
#1431=LINE('',#7533,#1758);
#1432=LINE('',#7536,#1759);
#1433=LINE('',#7538,#1760);
#1434=LINE('',#7539,#1761);
#1435=LINE('',#7542,#1762);
#1436=LINE('',#7544,#1763);
#1437=LINE('',#7545,#1764);
#1438=LINE('',#7548,#1765);
#1439=LINE('',#7550,#1766);
#1440=LINE('',#7551,#1767);
#1441=LINE('',#7553,#1768);
#1442=LINE('',#7554,#1769);
#1443=LINE('',#7566,#1770);
#1444=LINE('',#7570,#1771);
#1445=LINE('',#7574,#1772);
#1446=LINE('',#7581,#1773);
#1447=LINE('',#7583,#1774);
#1448=LINE('',#7624,#1775);
#1449=LINE('',#7631,#1776);
#1450=LINE('',#7637,#1777);
#1451=LINE('',#7639,#1778);
#1452=LINE('',#7641,#1779);
#1453=LINE('',#7642,#1780);
#1454=LINE('',#7647,#1781);
#1455=LINE('',#7648,#1782);
#1456=LINE('',#7651,#1783);
#1457=LINE('',#7653,#1784);
#1458=LINE('',#7654,#1785);
#1459=LINE('',#7656,#1786);
#1460=LINE('',#7662,#1787);
#1461=LINE('',#7664,#1788);
#1462=LINE('',#7666,#1789);
#1463=LINE('',#7667,#1790);
#1464=LINE('',#7672,#1791);
#1465=LINE('',#7673,#1792);
#1466=LINE('',#7676,#1793);
#1467=LINE('',#7678,#1794);
#1468=LINE('',#7679,#1795);
#1469=LINE('',#7681,#1796);
#1470=LINE('',#7688,#1797);
#1471=LINE('',#7696,#1798);
#1472=LINE('',#7713,#1799);
#1473=LINE('',#7764,#1800);
#1474=LINE('',#7768,#1801);
#1475=LINE('',#7770,#1802);
#1476=LINE('',#7772,#1803);
#1477=LINE('',#7773,#1804);
#1478=LINE('',#7776,#1805);
#1479=LINE('',#7778,#1806);
#1480=LINE('',#7779,#1807);
#1481=LINE('',#7782,#1808);
#1482=LINE('',#7784,#1809);
#1483=LINE('',#7785,#1810);
#1484=LINE('',#7794,#1811);
#1485=LINE('',#7801,#1812);
#1486=LINE('',#7818,#1813);
#1487=LINE('',#7869,#1814);
#1488=LINE('',#7873,#1815);
#1489=LINE('',#7875,#1816);
#1490=LINE('',#7877,#1817);
#1491=LINE('',#7878,#1818);
#1492=LINE('',#7881,#1819);
#1493=LINE('',#7883,#1820);
#1494=LINE('',#7884,#1821);
#1495=LINE('',#7887,#1822);
#1496=LINE('',#7889,#1823);
#1497=LINE('',#7890,#1824);
#1498=LINE('',#7899,#1825);
#1499=LINE('',#7906,#1826);
#1500=LINE('',#7927,#1827);
#1501=LINE('',#7982,#1828);
#1502=LINE('',#7987,#1829);
#1503=LINE('',#7993,#1830);
#1504=LINE('',#8001,#1831);
#1505=LINE('',#8022,#1832);
#1506=LINE('',#8077,#1833);
#1507=LINE('',#8082,#1834);
#1508=LINE('',#8088,#1835);
#1509=LINE('',#8097,#1836);
#1510=LINE('',#8103,#1837);
#1511=LINE('',#8112,#1838);
#1512=LINE('',#8118,#1839);
#1513=LINE('',#8126,#1840);
#1514=LINE('',#8128,#1841);
#1515=LINE('',#8130,#1842);
#1516=LINE('',#8132,#1843);
#1517=LINE('',#8134,#1844);
#1518=LINE('',#8136,#1845);
#1519=LINE('',#8138,#1846);
#1520=LINE('',#8139,#1847);
#1521=LINE('',#8142,#1848);
#1522=LINE('',#8144,#1849);
#1523=LINE('',#8145,#1850);
#1524=LINE('',#8148,#1851);
#1525=LINE('',#8149,#1852);
#1526=LINE('',#8152,#1853);
#1527=LINE('',#8153,#1854);
#1528=LINE('',#8156,#1855);
#1529=LINE('',#8157,#1856);
#1530=LINE('',#8161,#1857);
#1531=LINE('',#8162,#1858);
#1532=LINE('',#8164,#1859);
#1533=LINE('',#8165,#1860);
#1534=LINE('',#8167,#1861);
#1535=LINE('',#8169,#1862);
#1536=LINE('',#8171,#1863);
#1537=LINE('',#8177,#1864);
#1538=LINE('',#8179,#1865);
#1539=LINE('',#8181,#1866);
#1540=LINE('',#8182,#1867);
#1541=LINE('',#8185,#1868);
#1542=LINE('',#8187,#1869);
#1543=LINE('',#8188,#1870);
#1544=LINE('',#8191,#1871);
#1545=LINE('',#8193,#1872);
#1546=LINE('',#8194,#1873);
#1547=LINE('',#8197,#1874);
#1548=LINE('',#8199,#1875);
#1549=LINE('',#8200,#1876);
#1550=LINE('',#8203,#1877);
#1551=LINE('',#8205,#1878);
#1552=LINE('',#8206,#1879);
#1553=LINE('',#8208,#1880);
#1554=LINE('',#8209,#1881);
#1555=LINE('',#8217,#1882);
#1556=LINE('',#8221,#1883);
#1557=LINE('',#8225,#1884);
#1558=LINE('',#8234,#1885);
#1559=LINE('',#8238,#1886);
#1560=LINE('',#8242,#1887);
#1561=LINE('',#8249,#1888);
#1562=LINE('',#8253,#1889);
#1563=LINE('',#8257,#1890);
#1564=LINE('',#8262,#1891);
#1565=LINE('',#8264,#1892);
#1566=LINE('',#8266,#1893);
#1567=LINE('',#8267,#1894);
#1568=LINE('',#8270,#1895);
#1569=LINE('',#8272,#1896);
#1570=LINE('',#8273,#1897);
#1571=LINE('',#8276,#1898);
#1572=LINE('',#8278,#1899);
#1573=LINE('',#8279,#1900);
#1574=LINE('',#8282,#1901);
#1575=LINE('',#8284,#1902);
#1576=LINE('',#8285,#1903);
#1577=LINE('',#8288,#1904);
#1578=LINE('',#8290,#1905);
#1579=LINE('',#8291,#1906);
#1580=LINE('',#8293,#1907);
#1581=LINE('',#8294,#1908);
#1582=VECTOR('',#5158,0.33);
#1583=VECTOR('',#5165,0.33);
#1584=VECTOR('',#5172,0.33);
#1585=VECTOR('',#5179,0.33);
#1586=VECTOR('',#5186,0.34);
#1587=VECTOR('',#5193,0.34);
#1588=VECTOR('',#5200,0.34);
#1589=VECTOR('',#5207,0.34);
#1590=VECTOR('',#5214,0.34);
#1591=VECTOR('',#5221,0.34);
#1592=VECTOR('',#5226,1.);
#1593=VECTOR('',#5227,1.);
#1594=VECTOR('',#5228,1.);
#1595=VECTOR('',#5229,1.);
#1596=VECTOR('',#5232,1.);
#1597=VECTOR('',#5233,1.);
#1598=VECTOR('',#5234,1.);
#1599=VECTOR('',#5237,1.);
#1600=VECTOR('',#5238,1.);
#1601=VECTOR('',#5239,1.);
#1602=VECTOR('',#5242,1.);
#1603=VECTOR('',#5243,1.);
#1604=VECTOR('',#5254,0.25);
#1605=VECTOR('',#5263,0.25);
#1606=VECTOR('',#5270,1.);
#1607=VECTOR('',#5271,1.);
#1608=VECTOR('',#5272,1.);
#1609=VECTOR('',#5273,1.);
#1610=VECTOR('',#5276,1.);
#1611=VECTOR('',#5277,1.);
#1612=VECTOR('',#5278,1.);
#1613=VECTOR('',#5281,1.);
#1614=VECTOR('',#5282,1.);
#1615=VECTOR('',#5283,1.);
#1616=VECTOR('',#5286,1.);
#1617=VECTOR('',#5287,1.);
#1618=VECTOR('',#5296,1.);
#1619=VECTOR('',#5297,1.);
#1620=VECTOR('',#5298,1.);
#1621=VECTOR('',#5299,1.);
#1622=VECTOR('',#5302,1.);
#1623=VECTOR('',#5303,1.);
#1624=VECTOR('',#5304,1.);
#1625=VECTOR('',#5307,1.);
#1626=VECTOR('',#5308,1.);
#1627=VECTOR('',#5309,1.);
#1628=VECTOR('',#5312,1.);
#1629=VECTOR('',#5313,1.);
#1630=VECTOR('',#5324,0.25);
#1631=VECTOR('',#5333,0.25);
#1632=VECTOR('',#5340,1.);
#1633=VECTOR('',#5341,1.);
#1634=VECTOR('',#5342,1.);
#1635=VECTOR('',#5343,1.);
#1636=VECTOR('',#5346,1.);
#1637=VECTOR('',#5347,1.);
#1638=VECTOR('',#5348,1.);
#1639=VECTOR('',#5351,1.);
#1640=VECTOR('',#5352,1.);
#1641=VECTOR('',#5353,1.);
#1642=VECTOR('',#5356,1.);
#1643=VECTOR('',#5357,1.);
#1644=VECTOR('',#5366,1.);
#1645=VECTOR('',#5367,1.);
#1646=VECTOR('',#5368,1.);
#1647=VECTOR('',#5369,1.);
#1648=VECTOR('',#5372,1.);
#1649=VECTOR('',#5373,1.);
#1650=VECTOR('',#5374,1.);
#1651=VECTOR('',#5377,1.);
#1652=VECTOR('',#5378,1.);
#1653=VECTOR('',#5379,1.);
#1654=VECTOR('',#5382,1.);
#1655=VECTOR('',#5383,1.);
#1656=VECTOR('',#5394,0.425);
#1657=VECTOR('',#5401,0.645);
#1658=VECTOR('',#5414,0.425);
#1659=VECTOR('',#5421,0.645);
#1660=VECTOR('',#5434,0.425);
#1661=VECTOR('',#5441,0.645);
#1662=VECTOR('',#5454,0.425);
#1663=VECTOR('',#5461,0.645);
#1664=VECTOR('',#5474,0.425);
#1665=VECTOR('',#5481,0.645);
#1666=VECTOR('',#5494,0.425);
#1667=VECTOR('',#5501,0.645);
#1668=VECTOR('',#5514,0.32);
#1669=VECTOR('',#5521,0.6);
#1670=VECTOR('',#5538,0.475);
#1671=VECTOR('',#5543,0.5);
#1672=VECTOR('',#5548,0.485);
#1673=VECTOR('',#5557,0.31);
#1674=VECTOR('',#5562,0.3);
#1675=VECTOR('',#5567,0.27);
#1676=VECTOR('',#5572,1.);
#1677=VECTOR('',#5573,1.);
#1678=VECTOR('',#5574,1.);
#1679=VECTOR('',#5575,1.);
#1680=VECTOR('',#5578,1.);
#1681=VECTOR('',#5579,1.);
#1682=VECTOR('',#5580,1.);
#1683=VECTOR('',#5583,1.);
#1684=VECTOR('',#5584,1.);
#1685=VECTOR('',#5585,1.);
#1686=VECTOR('',#5588,1.);
#1687=VECTOR('',#5589,1.);
#1688=VECTOR('',#5590,1.);
#1689=VECTOR('',#5593,1.);
#1690=VECTOR('',#5594,1.);
#1691=VECTOR('',#5595,1.);
#1692=VECTOR('',#5598,1.);
#1693=VECTOR('',#5599,1.);
#1694=VECTOR('',#5612,2.05);
#1695=VECTOR('',#5619,2.05);
#1696=VECTOR('',#5628,1.);
#1697=VECTOR('',#5629,1.);
#1698=VECTOR('',#5634,1.);
#1699=VECTOR('',#5637,1.);
#1700=VECTOR('',#5640,1.);
#1701=VECTOR('',#5643,1.);
#1702=VECTOR('',#5646,1.);
#1703=VECTOR('',#5647,1.);
#1704=VECTOR('',#5650,1.);
#1705=VECTOR('',#5651,1.);
#1706=VECTOR('',#5656,1.);
#1707=VECTOR('',#5657,1.);
#1708=VECTOR('',#5660,1.);
#1709=VECTOR('',#5661,1.);
#1710=VECTOR('',#5662,1.);
#1711=VECTOR('',#5663,1.);
#1712=VECTOR('',#5668,1.);
#1713=VECTOR('',#5669,1.);
#1714=VECTOR('',#5670,1.);
#1715=VECTOR('',#5671,1.);
#1716=VECTOR('',#5672,1.);
#1717=VECTOR('',#5673,1.);
#1718=VECTOR('',#5686,1.);
#1719=VECTOR('',#5687,1.);
#1720=VECTOR('',#5688,1.);
#1721=VECTOR('',#5689,1.);
#1722=VECTOR('',#5692,1.);
#1723=VECTOR('',#5693,1.);
#1724=VECTOR('',#5694,1.);
#1725=VECTOR('',#5697,1.);
#1726=VECTOR('',#5698,1.);
#1727=VECTOR('',#5699,1.);
#1728=VECTOR('',#5702,1.);
#1729=VECTOR('',#5703,1.);
#1730=VECTOR('',#5710,0.65);
#1731=VECTOR('',#5715,0.65);
#1732=VECTOR('',#5718,1.);
#1733=VECTOR('',#5719,1.);
#1734=VECTOR('',#5720,1.);
#1735=VECTOR('',#5723,1.);
#1736=VECTOR('',#5724,1.);
#1737=VECTOR('',#5727,1.);
#1738=VECTOR('',#5728,1.);
#1739=VECTOR('',#5731,1.);
#1740=VECTOR('',#5740,1.8);
#1741=VECTOR('',#5757,0.25);
#1742=VECTOR('',#5760,0.25);
#1743=VECTOR('',#5765,1.65);
#1744=VECTOR('',#5770,0.25);
#1745=VECTOR('',#5773,0.25);
#1746=VECTOR('',#5776,0.25);
#1747=VECTOR('',#5779,0.25);
#1748=VECTOR('',#5792,1.75);
#1749=VECTOR('',#5799,1.);
#1750=VECTOR('',#5810,0.42);
#1751=VECTOR('',#5817,0.8);
#1752=VECTOR('',#5828,1.);
#1753=VECTOR('',#5829,1.);
#1754=VECTOR('',#5830,1.);
#1755=VECTOR('',#5831,1.);
#1756=VECTOR('',#5834,1.);
#1757=VECTOR('',#5835,1.);
#1758=VECTOR('',#5836,1.);
#1759=VECTOR('',#5839,1.);
#1760=VECTOR('',#5840,1.);
#1761=VECTOR('',#5841,1.);
#1762=VECTOR('',#5844,1.);
#1763=VECTOR('',#5845,1.);
#1764=VECTOR('',#5846,1.);
#1765=VECTOR('',#5849,1.);
#1766=VECTOR('',#5850,1.);
#1767=VECTOR('',#5851,1.);
#1768=VECTOR('',#5854,1.);
#1769=VECTOR('',#5855,1.);
#1770=VECTOR('',#5872,0.625);
#1771=VECTOR('',#5877,0.65);
#1772=VECTOR('',#5882,0.635);
#1773=VECTOR('',#5891,0.41);
#1774=VECTOR('',#5894,0.4);
#1775=VECTOR('',#5971,0.21);
#1776=VECTOR('',#5980,0.21);
#1777=VECTOR('',#5987,1.);
#1778=VECTOR('',#5988,1.);
#1779=VECTOR('',#5989,1.);
#1780=VECTOR('',#5990,1.);
#1781=VECTOR('',#5995,1.);
#1782=VECTOR('',#5996,1.);
#1783=VECTOR('',#5999,1.);
#1784=VECTOR('',#6000,1.);
#1785=VECTOR('',#6001,1.);
#1786=VECTOR('',#6004,1.);
#1787=VECTOR('',#6011,1.);
#1788=VECTOR('',#6012,1.);
#1789=VECTOR('',#6013,1.);
#1790=VECTOR('',#6014,1.);
#1791=VECTOR('',#6019,1.);
#1792=VECTOR('',#6020,1.);
#1793=VECTOR('',#6023,1.);
#1794=VECTOR('',#6024,1.);
#1795=VECTOR('',#6025,1.);
#1796=VECTOR('',#6028,1.);
#1797=VECTOR('',#6037,1.);
#1798=VECTOR('',#6048,1.);
#1799=VECTOR('',#6055,0.21);
#1800=VECTOR('',#6060,1.);
#1801=VECTOR('',#6063,1.);
#1802=VECTOR('',#6064,1.);
#1803=VECTOR('',#6065,1.);
#1804=VECTOR('',#6066,1.);
#1805=VECTOR('',#6069,1.);
#1806=VECTOR('',#6070,1.);
#1807=VECTOR('',#6071,1.);
#1808=VECTOR('',#6074,1.);
#1809=VECTOR('',#6075,1.);
#1810=VECTOR('',#6076,1.);
#1811=VECTOR('',#6089,2.);
#1812=VECTOR('',#6098,1.);
#1813=VECTOR('',#6105,0.21);
#1814=VECTOR('',#6110,1.);
#1815=VECTOR('',#6113,1.);
#1816=VECTOR('',#6114,1.);
#1817=VECTOR('',#6115,1.);
#1818=VECTOR('',#6116,1.);
#1819=VECTOR('',#6119,1.);
#1820=VECTOR('',#6120,1.);
#1821=VECTOR('',#6121,1.);
#1822=VECTOR('',#6124,1.);
#1823=VECTOR('',#6125,1.);
#1824=VECTOR('',#6126,1.);
#1825=VECTOR('',#6139,2.);
#1826=VECTOR('',#6148,1.);
#1827=VECTOR('',#6155,0.21);
#1828=VECTOR('',#6160,1.);
#1829=VECTOR('',#6165,1.005);
#1830=VECTOR('',#6172,1.5);
#1831=VECTOR('',#6183,1.);
#1832=VECTOR('',#6190,0.21);
#1833=VECTOR('',#6195,1.);
#1834=VECTOR('',#6200,1.005);
#1835=VECTOR('',#6207,1.5);
#1836=VECTOR('',#6220,0.275);
#1837=VECTOR('',#6227,1.1);
#1838=VECTOR('',#6240,0.275);
#1839=VECTOR('',#6247,1.1);
#1840=VECTOR('',#6258,1.);
#1841=VECTOR('',#6259,1.);
#1842=VECTOR('',#6260,1.);
#1843=VECTOR('',#6261,1.);
#1844=VECTOR('',#6262,1.);
#1845=VECTOR('',#6263,1.);
#1846=VECTOR('',#6264,1.);
#1847=VECTOR('',#6265,1.);
#1848=VECTOR('',#6268,1.);
#1849=VECTOR('',#6269,1.);
#1850=VECTOR('',#6270,1.);
#1851=VECTOR('',#6273,1.);
#1852=VECTOR('',#6274,1.);
#1853=VECTOR('',#6277,1.);
#1854=VECTOR('',#6278,1.);
#1855=VECTOR('',#6281,1.);
#1856=VECTOR('',#6282,1.);
#1857=VECTOR('',#6285,1.);
#1858=VECTOR('',#6286,1.);
#1859=VECTOR('',#6287,1.);
#1860=VECTOR('',#6288,1.);
#1861=VECTOR('',#6291,1.);
#1862=VECTOR('',#6294,1.);
#1863=VECTOR('',#6297,1.);
#1864=VECTOR('',#6304,1.);
#1865=VECTOR('',#6305,1.);
#1866=VECTOR('',#6306,1.);
#1867=VECTOR('',#6307,1.);
#1868=VECTOR('',#6310,1.);
#1869=VECTOR('',#6311,1.);
#1870=VECTOR('',#6312,1.);
#1871=VECTOR('',#6315,1.);
#1872=VECTOR('',#6316,1.);
#1873=VECTOR('',#6317,1.);
#1874=VECTOR('',#6320,1.);
#1875=VECTOR('',#6321,1.);
#1876=VECTOR('',#6322,1.);
#1877=VECTOR('',#6325,1.);
#1878=VECTOR('',#6326,1.);
#1879=VECTOR('',#6327,1.);
#1880=VECTOR('',#6330,1.);
#1881=VECTOR('',#6331,1.);
#1882=VECTOR('',#6342,0.235);
#1883=VECTOR('',#6347,0.25);
#1884=VECTOR('',#6352,0.2125);
#1885=VECTOR('',#6365,0.4);
#1886=VECTOR('',#6370,0.425);
#1887=VECTOR('',#6375,0.41);
#1888=VECTOR('',#6384,0.26);
#1889=VECTOR('',#6389,0.25);
#1890=VECTOR('',#6394,0.225);
#1891=VECTOR('',#6399,1.);
#1892=VECTOR('',#6400,1.);
#1893=VECTOR('',#6401,1.);
#1894=VECTOR('',#6402,1.);
#1895=VECTOR('',#6405,1.);
#1896=VECTOR('',#6406,1.);
#1897=VECTOR('',#6407,1.);
#1898=VECTOR('',#6410,1.);
#1899=VECTOR('',#6411,1.);
#1900=VECTOR('',#6412,1.);
#1901=VECTOR('',#6415,1.);
#1902=VECTOR('',#6416,1.);
#1903=VECTOR('',#6417,1.);
#1904=VECTOR('',#6420,1.);
#1905=VECTOR('',#6421,1.);
#1906=VECTOR('',#6422,1.);
#1907=VECTOR('',#6425,1.);
#1908=VECTOR('',#6426,1.);
#1909=CIRCLE('',#4657,0.33);
#1910=CIRCLE('',#4658,0.33);
#1911=CIRCLE('',#4660,0.33);
#1912=CIRCLE('',#4661,0.33);
#1913=CIRCLE('',#4663,0.33);
#1914=CIRCLE('',#4664,0.33);
#1915=CIRCLE('',#4666,0.33);
#1916=CIRCLE('',#4667,0.33);
#1917=CIRCLE('',#4669,0.34);
#1918=CIRCLE('',#4670,0.34);
#1919=CIRCLE('',#4672,0.34);
#1920=CIRCLE('',#4673,0.34);
#1921=CIRCLE('',#4675,0.34);
#1922=CIRCLE('',#4676,0.34);
#1923=CIRCLE('',#4678,0.34);
#1924=CIRCLE('',#4679,0.34);
#1925=CIRCLE('',#4681,0.34);
#1926=CIRCLE('',#4682,0.34);
#1927=CIRCLE('',#4684,0.34);
#1928=CIRCLE('',#4685,0.34);
#1929=CIRCLE('',#4694,0.25);
#1930=CIRCLE('',#4695,0.25);
#1931=CIRCLE('',#4698,0.25);
#1932=CIRCLE('',#4699,0.25);
#1933=CIRCLE('',#4716,0.25);
#1934=CIRCLE('',#4717,0.25);
#1935=CIRCLE('',#4720,0.25);
#1936=CIRCLE('',#4721,0.25);
#1937=CIRCLE('',#4738,0.425);
#1938=CIRCLE('',#4739,0.425);
#1939=CIRCLE('',#4741,0.645);
#1940=CIRCLE('',#4742,0.645);
#1941=CIRCLE('',#4747,0.425);
#1942=CIRCLE('',#4748,0.425);
#1943=CIRCLE('',#4750,0.645);
#1944=CIRCLE('',#4751,0.645);
#1945=CIRCLE('',#4756,0.425);
#1946=CIRCLE('',#4757,0.425);
#1947=CIRCLE('',#4759,0.645);
#1948=CIRCLE('',#4760,0.645);
#1949=CIRCLE('',#4765,0.425);
#1950=CIRCLE('',#4766,0.425);
#1951=CIRCLE('',#4768,0.645);
#1952=CIRCLE('',#4769,0.645);
#1953=CIRCLE('',#4774,0.425);
#1954=CIRCLE('',#4775,0.425);
#1955=CIRCLE('',#4777,0.645);
#1956=CIRCLE('',#4778,0.645);
#1957=CIRCLE('',#4783,0.425);
#1958=CIRCLE('',#4784,0.425);
#1959=CIRCLE('',#4786,0.645);
#1960=CIRCLE('',#4787,0.645);
#1961=CIRCLE('',#4792,0.32);
#1962=CIRCLE('',#4793,0.32);
#1963=CIRCLE('',#4795,0.6);
#1964=CIRCLE('',#4796,0.6);
#1965=CIRCLE('',#4801,0.45);
#1966=CIRCLE('',#4803,0.5);
#1967=CIRCLE('',#4805,0.5);
#1968=CIRCLE('',#4807,0.47);
#1969=CIRCLE('',#4809,0.32);
#1970=CIRCLE('',#4811,0.2942);
#1971=CIRCLE('',#4813,0.2942);
#1972=CIRCLE('',#4815,0.24);
#1973=CIRCLE('',#4828,2.05);
#1974=CIRCLE('',#4829,2.05);
#1975=CIRCLE('',#4831,2.05);
#1976=CIRCLE('',#4832,2.05);
#1977=CIRCLE('',#4834,2.35);
#1978=CIRCLE('',#4836,2.8);
#1979=CIRCLE('',#4838,2.8);
#1980=CIRCLE('',#4840,2.8);
#1981=CIRCLE('',#4843,2.8);
#1982=CIRCLE('',#4846,0.65);
#1983=CIRCLE('',#4847,0.65);
#1984=CIRCLE('',#4849,2.8);
#1985=CIRCLE('',#4850,2.8);
#1986=CIRCLE('',#4859,0.65);
#1987=CIRCLE('',#4861,0.65);
#1988=CIRCLE('',#4869,1.8);
#1989=CIRCLE('',#4870,1.8);
#1990=CIRCLE('',#4872,2.19089023002066);
#1991=CIRCLE('',#4874,2.35);
#1992=CIRCLE('',#4875,2.19089023002066);
#1993=CIRCLE('',#4880,1.65);
#1994=CIRCLE('',#4881,1.65);
#1995=CIRCLE('',#4887,1.);
#1996=CIRCLE('',#4889,1.75);
#1997=CIRCLE('',#4891,1.75);
#1998=CIRCLE('',#4893,1.);
#1999=CIRCLE('',#4899,0.42);
#2000=CIRCLE('',#4900,0.42);
#2001=CIRCLE('',#4902,0.8);
#2002=CIRCLE('',#4903,0.8);
#2003=CIRCLE('',#4916,0.3933);
#2004=CIRCLE('',#4918,0.6);
#2005=CIRCLE('',#4920,0.65);
#2006=CIRCLE('',#4922,0.65);
#2007=CIRCLE('',#4924,0.62);
#2008=CIRCLE('',#4926,0.42);
#2009=CIRCLE('',#4928,0.3933);
#2010=CIRCLE('',#4967,0.21);
#2011=CIRCLE('',#4968,0.21);
#2012=CIRCLE('',#4971,0.21);
#2013=CIRCLE('',#4972,0.21);
#2014=CIRCLE('',#4976,1.);
#2015=CIRCLE('',#4980,1.);
#2016=CIRCLE('',#4983,1.);
#2017=CIRCLE('',#4987,1.);
#2018=CIRCLE('',#4989,1.);
#2019=CIRCLE('',#4990,1.);
#2020=CIRCLE('',#4995,0.21);
#2021=CIRCLE('',#4997,0.21);
#2022=CIRCLE('',#4998,0.21);
#2023=CIRCLE('',#5004,2.);
#2024=CIRCLE('',#5005,1.);
#2025=CIRCLE('',#5007,1.);
#2026=CIRCLE('',#5009,2.);
#2027=CIRCLE('',#5013,0.21);
#2028=CIRCLE('',#5015,0.21);
#2029=CIRCLE('',#5016,0.21);
#2030=CIRCLE('',#5022,2.);
#2031=CIRCLE('',#5023,1.);
#2032=CIRCLE('',#5025,1.);
#2033=CIRCLE('',#5027,2.);
#2034=CIRCLE('',#5031,0.21);
#2035=CIRCLE('',#5033,0.21);
#2036=CIRCLE('',#5034,0.21);
#2037=CIRCLE('',#5037,1.005);
#2038=CIRCLE('',#5038,1.005);
#2039=CIRCLE('',#5040,1.5);
#2040=CIRCLE('',#5041,1.5);
#2041=CIRCLE('',#5046,0.21);
#2042=CIRCLE('',#5048,0.21);
#2043=CIRCLE('',#5049,0.21);
#2044=CIRCLE('',#5052,1.005);
#2045=CIRCLE('',#5053,1.005);
#2046=CIRCLE('',#5055,1.5);
#2047=CIRCLE('',#5056,1.5);
#2048=CIRCLE('',#5061,0.275);
#2049=CIRCLE('',#5062,0.275);
#2050=CIRCLE('',#5064,1.1);
#2051=CIRCLE('',#5065,1.1);
#2052=CIRCLE('',#5070,0.275);
#2053=CIRCLE('',#5071,0.275);
#2054=CIRCLE('',#5073,1.1);
#2055=CIRCLE('',#5074,1.1);
#2056=CIRCLE('',#5097,0.22);
#2057=CIRCLE('',#5099,0.24505);
#2058=CIRCLE('',#5101,0.24505);
#2059=CIRCLE('',#5103,0.175);
#2060=CIRCLE('',#5107,0.375);
#2061=CIRCLE('',#5109,0.425);
#2062=CIRCLE('',#5111,0.425);
#2063=CIRCLE('',#5113,0.395);
#2064=CIRCLE('',#5115,0.27);
#2065=CIRCLE('',#5117,0.24505);
#2066=CIRCLE('',#5119,0.24505);
#2067=CIRCLE('',#5121,0.2);
#2068=VERTEX_POINT('',#6469);
#2069=VERTEX_POINT('',#6471);
#2070=VERTEX_POINT('',#6475);
#2071=VERTEX_POINT('',#6477);
#2072=VERTEX_POINT('',#6481);
#2073=VERTEX_POINT('',#6483);
#2074=VERTEX_POINT('',#6487);
#2075=VERTEX_POINT('',#6489);
#2076=VERTEX_POINT('',#6493);
#2077=VERTEX_POINT('',#6495);
#2078=VERTEX_POINT('',#6499);
#2079=VERTEX_POINT('',#6501);
#2080=VERTEX_POINT('',#6505);
#2081=VERTEX_POINT('',#6507);
#2082=VERTEX_POINT('',#6511);
#2083=VERTEX_POINT('',#6513);
#2084=VERTEX_POINT('',#6517);
#2085=VERTEX_POINT('',#6519);
#2086=VERTEX_POINT('',#6523);
#2087=VERTEX_POINT('',#6525);
#2088=VERTEX_POINT('',#6529);
#2089=VERTEX_POINT('',#6530);
#2090=VERTEX_POINT('',#6532);
#2091=VERTEX_POINT('',#6534);
#2092=VERTEX_POINT('',#6538);
#2093=VERTEX_POINT('',#6540);
#2094=VERTEX_POINT('',#6544);
#2095=VERTEX_POINT('',#6546);
#2096=VERTEX_POINT('',#6556);
#2097=VERTEX_POINT('',#6558);
#2098=VERTEX_POINT('',#6563);
#2099=VERTEX_POINT('',#6565);
#2100=VERTEX_POINT('',#6570);
#2101=VERTEX_POINT('',#6571);
#2102=VERTEX_POINT('',#6573);
#2103=VERTEX_POINT('',#6575);
#2104=VERTEX_POINT('',#6579);
#2105=VERTEX_POINT('',#6581);
#2106=VERTEX_POINT('',#6585);
#2107=VERTEX_POINT('',#6587);
#2108=VERTEX_POINT('',#6597);
#2109=VERTEX_POINT('',#6598);
#2110=VERTEX_POINT('',#6600);
#2111=VERTEX_POINT('',#6602);
#2112=VERTEX_POINT('',#6606);
#2113=VERTEX_POINT('',#6608);
#2114=VERTEX_POINT('',#6612);
#2115=VERTEX_POINT('',#6614);
#2116=VERTEX_POINT('',#6624);
#2117=VERTEX_POINT('',#6626);
#2118=VERTEX_POINT('',#6631);
#2119=VERTEX_POINT('',#6633);
#2120=VERTEX_POINT('',#6638);
#2121=VERTEX_POINT('',#6639);
#2122=VERTEX_POINT('',#6641);
#2123=VERTEX_POINT('',#6643);
#2124=VERTEX_POINT('',#6647);
#2125=VERTEX_POINT('',#6649);
#2126=VERTEX_POINT('',#6653);
#2127=VERTEX_POINT('',#6655);
#2128=VERTEX_POINT('',#6665);
#2129=VERTEX_POINT('',#6666);
#2130=VERTEX_POINT('',#6668);
#2131=VERTEX_POINT('',#6670);
#2132=VERTEX_POINT('',#6674);
#2133=VERTEX_POINT('',#6676);
#2134=VERTEX_POINT('',#6680);
#2135=VERTEX_POINT('',#6682);
#2136=VERTEX_POINT('',#6692);
#2137=VERTEX_POINT('',#6694);
#2138=VERTEX_POINT('',#6698);
#2139=VERTEX_POINT('',#6700);
#2140=VERTEX_POINT('',#6707);
#2141=VERTEX_POINT('',#6709);
#2142=VERTEX_POINT('',#6713);
#2143=VERTEX_POINT('',#6715);
#2144=VERTEX_POINT('',#6722);
#2145=VERTEX_POINT('',#6724);
#2146=VERTEX_POINT('',#6728);
#2147=VERTEX_POINT('',#6730);
#2148=VERTEX_POINT('',#6737);
#2149=VERTEX_POINT('',#6739);
#2150=VERTEX_POINT('',#6743);
#2151=VERTEX_POINT('',#6745);
#2152=VERTEX_POINT('',#6752);
#2153=VERTEX_POINT('',#6754);
#2154=VERTEX_POINT('',#6758);
#2155=VERTEX_POINT('',#6760);
#2156=VERTEX_POINT('',#6767);
#2157=VERTEX_POINT('',#6769);
#2158=VERTEX_POINT('',#6773);
#2159=VERTEX_POINT('',#6775);
#2160=VERTEX_POINT('',#6782);
#2161=VERTEX_POINT('',#6784);
#2162=VERTEX_POINT('',#6788);
#2163=VERTEX_POINT('',#6790);
#2164=VERTEX_POINT('',#6797);
#2165=VERTEX_POINT('',#6800);
#2166=VERTEX_POINT('',#6804);
#2167=VERTEX_POINT('',#6808);
#2168=VERTEX_POINT('',#6812);
#2169=VERTEX_POINT('',#6815);
#2170=VERTEX_POINT('',#6819);
#2171=VERTEX_POINT('',#6823);
#2172=VERTEX_POINT('',#6828);
#2173=VERTEX_POINT('',#6829);
#2174=VERTEX_POINT('',#6831);
#2175=VERTEX_POINT('',#6833);
#2176=VERTEX_POINT('',#6837);
#2177=VERTEX_POINT('',#6839);
#2178=VERTEX_POINT('',#6843);
#2179=VERTEX_POINT('',#6845);
#2180=VERTEX_POINT('',#6849);
#2181=VERTEX_POINT('',#6851);
#2182=VERTEX_POINT('',#6855);
#2183=VERTEX_POINT('',#6857);
#2184=VERTEX_POINT('',#6868);
#2185=VERTEX_POINT('',#6870);
#2186=VERTEX_POINT('',#6874);
#2187=VERTEX_POINT('',#6876);
#2188=VERTEX_POINT('',#6880);
#2189=VERTEX_POINT('',#6881);
#2190=VERTEX_POINT('',#6884);
#2191=VERTEX_POINT('',#6885);
#2192=VERTEX_POINT('',#6887);
#2193=VERTEX_POINT('',#6891);
#2194=VERTEX_POINT('',#6892);
#2195=VERTEX_POINT('',#6894);
#2196=VERTEX_POINT('',#6898);
#2197=VERTEX_POINT('',#6899);
#2198=VERTEX_POINT('',#6901);
#2199=VERTEX_POINT('',#6908);
#2200=VERTEX_POINT('',#6909);
#2201=VERTEX_POINT('',#6911);
#2202=VERTEX_POINT('',#6918);
#2203=VERTEX_POINT('',#6919);
#2204=VERTEX_POINT('',#6921);
#2205=VERTEX_POINT('',#6923);
#2206=VERTEX_POINT('',#6926);
#2207=VERTEX_POINT('',#6928);
#2208=VERTEX_POINT('',#6930);
#2209=VERTEX_POINT('',#6932);
#2210=VERTEX_POINT('',#6935);
#2211=VERTEX_POINT('',#6937);
#2212=VERTEX_POINT('',#6946);
#2213=VERTEX_POINT('',#6947);
#2214=VERTEX_POINT('',#6949);
#2215=VERTEX_POINT('',#6951);
#2216=VERTEX_POINT('',#6955);
#2217=VERTEX_POINT('',#6957);
#2218=VERTEX_POINT('',#6961);
#2219=VERTEX_POINT('',#6963);
#2220=VERTEX_POINT('',#6971);
#2221=VERTEX_POINT('',#6975);
#2222=VERTEX_POINT('',#6979);
#2223=VERTEX_POINT('',#6980);
#2224=VERTEX_POINT('',#6985);
#2225=VERTEX_POINT('',#6989);
#2226=VERTEX_POINT('',#6997);
#2227=VERTEX_POINT('',#6999);
#2228=VERTEX_POINT('',#7003);
#2229=VERTEX_POINT('',#7006);
#2230=VERTEX_POINT('',#7007);
#2231=VERTEX_POINT('',#7009);
#2232=VERTEX_POINT('',#7013);
#2233=VERTEX_POINT('',#7014);
#2234=VERTEX_POINT('',#7025);
#2235=VERTEX_POINT('',#7054);
#2236=VERTEX_POINT('',#7091);
#2237=VERTEX_POINT('',#7126);
#2238=VERTEX_POINT('',#7128);
#2239=VERTEX_POINT('',#7139);
#2240=VERTEX_POINT('',#7169);
#2241=VERTEX_POINT('',#7171);
#2242=VERTEX_POINT('',#7174);
#2243=VERTEX_POINT('',#7175);
#2244=VERTEX_POINT('',#7194);
#2245=VERTEX_POINT('',#7215);
#2246=VERTEX_POINT('',#7216);
#2247=VERTEX_POINT('',#7235);
#2248=VERTEX_POINT('',#7256);
#2249=VERTEX_POINT('',#7257);
#2250=VERTEX_POINT('',#7276);
#2251=VERTEX_POINT('',#7297);
#2252=VERTEX_POINT('',#7298);
#2253=VERTEX_POINT('',#7317);
#2254=VERTEX_POINT('',#7339);
#2255=VERTEX_POINT('',#7376);
#2256=VERTEX_POINT('',#7413);
#2257=VERTEX_POINT('',#7450);
#2258=VERTEX_POINT('',#7487);
#2259=VERTEX_POINT('',#7490);
#2260=VERTEX_POINT('',#7493);
#2261=VERTEX_POINT('',#7497);
#2262=VERTEX_POINT('',#7505);
#2263=VERTEX_POINT('',#7507);
#2264=VERTEX_POINT('',#7511);
#2265=VERTEX_POINT('',#7513);
#2266=VERTEX_POINT('',#7520);
#2267=VERTEX_POINT('',#7521);
#2268=VERTEX_POINT('',#7523);
#2269=VERTEX_POINT('',#7525);
#2270=VERTEX_POINT('',#7529);
#2271=VERTEX_POINT('',#7531);
#2272=VERTEX_POINT('',#7535);
#2273=VERTEX_POINT('',#7537);
#2274=VERTEX_POINT('',#7541);
#2275=VERTEX_POINT('',#7543);
#2276=VERTEX_POINT('',#7547);
#2277=VERTEX_POINT('',#7549);
#2278=VERTEX_POINT('',#7558);
#2279=VERTEX_POINT('',#7561);
#2280=VERTEX_POINT('',#7564);
#2281=VERTEX_POINT('',#7568);
#2282=VERTEX_POINT('',#7572);
#2283=VERTEX_POINT('',#7576);
#2284=VERTEX_POINT('',#7579);
#2285=VERTEX_POINT('',#7621);
#2286=VERTEX_POINT('',#7623);
#2287=VERTEX_POINT('',#7628);
#2288=VERTEX_POINT('',#7630);
#2289=VERTEX_POINT('',#7635);
#2290=VERTEX_POINT('',#7636);
#2291=VERTEX_POINT('',#7638);
#2292=VERTEX_POINT('',#7640);
#2293=VERTEX_POINT('',#7644);
#2294=VERTEX_POINT('',#7646);
#2295=VERTEX_POINT('',#7650);
#2296=VERTEX_POINT('',#7652);
#2297=VERTEX_POINT('',#7660);
#2298=VERTEX_POINT('',#7661);
#2299=VERTEX_POINT('',#7663);
#2300=VERTEX_POINT('',#7665);
#2301=VERTEX_POINT('',#7669);
#2302=VERTEX_POINT('',#7671);
#2303=VERTEX_POINT('',#7675);
#2304=VERTEX_POINT('',#7677);
#2305=VERTEX_POINT('',#7685);
#2306=VERTEX_POINT('',#7687);
#2307=VERTEX_POINT('',#7694);
#2308=VERTEX_POINT('',#7695);
#2309=VERTEX_POINT('',#7699);
#2310=VERTEX_POINT('',#7710);
#2311=VERTEX_POINT('',#7712);
#2312=VERTEX_POINT('',#7714);
#2313=VERTEX_POINT('',#7751);
#2314=VERTEX_POINT('',#7766);
#2315=VERTEX_POINT('',#7767);
#2316=VERTEX_POINT('',#7769);
#2317=VERTEX_POINT('',#7771);
#2318=VERTEX_POINT('',#7775);
#2319=VERTEX_POINT('',#7777);
#2320=VERTEX_POINT('',#7781);
#2321=VERTEX_POINT('',#7783);
#2322=VERTEX_POINT('',#7787);
#2323=VERTEX_POINT('',#7793);
#2324=VERTEX_POINT('',#7799);
#2325=VERTEX_POINT('',#7800);
#2326=VERTEX_POINT('',#7804);
#2327=VERTEX_POINT('',#7815);
#2328=VERTEX_POINT('',#7817);
#2329=VERTEX_POINT('',#7819);
#2330=VERTEX_POINT('',#7856);
#2331=VERTEX_POINT('',#7871);
#2332=VERTEX_POINT('',#7872);
#2333=VERTEX_POINT('',#7874);
#2334=VERTEX_POINT('',#7876);
#2335=VERTEX_POINT('',#7880);
#2336=VERTEX_POINT('',#7882);
#2337=VERTEX_POINT('',#7886);
#2338=VERTEX_POINT('',#7888);
#2339=VERTEX_POINT('',#7892);
#2340=VERTEX_POINT('',#7898);
#2341=VERTEX_POINT('',#7904);
#2342=VERTEX_POINT('',#7905);
#2343=VERTEX_POINT('',#7909);
#2344=VERTEX_POINT('',#7924);
#2345=VERTEX_POINT('',#7926);
#2346=VERTEX_POINT('',#7928);
#2347=VERTEX_POINT('',#7965);
#2348=VERTEX_POINT('',#7984);
#2349=VERTEX_POINT('',#7986);
#2350=VERTEX_POINT('',#7990);
#2351=VERTEX_POINT('',#7992);
#2352=VERTEX_POINT('',#7999);
#2353=VERTEX_POINT('',#8000);
#2354=VERTEX_POINT('',#8004);
#2355=VERTEX_POINT('',#8019);
#2356=VERTEX_POINT('',#8021);
#2357=VERTEX_POINT('',#8023);
#2358=VERTEX_POINT('',#8060);
#2359=VERTEX_POINT('',#8079);
#2360=VERTEX_POINT('',#8081);
#2361=VERTEX_POINT('',#8085);
#2362=VERTEX_POINT('',#8087);
#2363=VERTEX_POINT('',#8094);
#2364=VERTEX_POINT('',#8096);
#2365=VERTEX_POINT('',#8100);
#2366=VERTEX_POINT('',#8102);
#2367=VERTEX_POINT('',#8109);
#2368=VERTEX_POINT('',#8111);
#2369=VERTEX_POINT('',#8115);
#2370=VERTEX_POINT('',#8117);
#2371=VERTEX_POINT('',#8124);
#2372=VERTEX_POINT('',#8125);
#2373=VERTEX_POINT('',#8127);
#2374=VERTEX_POINT('',#8129);
#2375=VERTEX_POINT('',#8131);
#2376=VERTEX_POINT('',#8133);
#2377=VERTEX_POINT('',#8135);
#2378=VERTEX_POINT('',#8137);
#2379=VERTEX_POINT('',#8141);
#2380=VERTEX_POINT('',#8143);
#2381=VERTEX_POINT('',#8147);
#2382=VERTEX_POINT('',#8151);
#2383=VERTEX_POINT('',#8155);
#2384=VERTEX_POINT('',#8159);
#2385=VERTEX_POINT('',#8160);
#2386=VERTEX_POINT('',#8163);
#2387=VERTEX_POINT('',#8175);
#2388=VERTEX_POINT('',#8176);
#2389=VERTEX_POINT('',#8178);
#2390=VERTEX_POINT('',#8180);
#2391=VERTEX_POINT('',#8184);
#2392=VERTEX_POINT('',#8186);
#2393=VERTEX_POINT('',#8190);
#2394=VERTEX_POINT('',#8192);
#2395=VERTEX_POINT('',#8196);
#2396=VERTEX_POINT('',#8198);
#2397=VERTEX_POINT('',#8202);
#2398=VERTEX_POINT('',#8204);
#2399=VERTEX_POINT('',#8212);
#2400=VERTEX_POINT('',#8215);
#2401=VERTEX_POINT('',#8219);
#2402=VERTEX_POINT('',#8223);
#2403=VERTEX_POINT('',#8229);
#2404=VERTEX_POINT('',#8232);
#2405=VERTEX_POINT('',#8236);
#2406=VERTEX_POINT('',#8240);
#2407=VERTEX_POINT('',#8244);
#2408=VERTEX_POINT('',#8247);
#2409=VERTEX_POINT('',#8251);
#2410=VERTEX_POINT('',#8255);
#2411=VERTEX_POINT('',#8260);
#2412=VERTEX_POINT('',#8261);
#2413=VERTEX_POINT('',#8263);
#2414=VERTEX_POINT('',#8265);
#2415=VERTEX_POINT('',#8269);
#2416=VERTEX_POINT('',#8271);
#2417=VERTEX_POINT('',#8275);
#2418=VERTEX_POINT('',#8277);
#2419=VERTEX_POINT('',#8281);
#2420=VERTEX_POINT('',#8283);
#2421=VERTEX_POINT('',#8287);
#2422=VERTEX_POINT('',#8289);
#2423=EDGE_CURVE('',#2068,#2068,#1909,.T.);
#2424=EDGE_CURVE('',#2068,#2069,#1255,.T.);
#2425=EDGE_CURVE('',#2069,#2069,#1910,.T.);
#2426=EDGE_CURVE('',#2070,#2070,#1911,.T.);
#2427=EDGE_CURVE('',#2070,#2071,#1256,.T.);
#2428=EDGE_CURVE('',#2071,#2071,#1912,.T.);
#2429=EDGE_CURVE('',#2072,#2072,#1913,.T.);
#2430=EDGE_CURVE('',#2072,#2073,#1257,.T.);
#2431=EDGE_CURVE('',#2073,#2073,#1914,.T.);
#2432=EDGE_CURVE('',#2074,#2074,#1915,.T.);
#2433=EDGE_CURVE('',#2074,#2075,#1258,.T.);
#2434=EDGE_CURVE('',#2075,#2075,#1916,.T.);
#2435=EDGE_CURVE('',#2076,#2076,#1917,.T.);
#2436=EDGE_CURVE('',#2076,#2077,#1259,.T.);
#2437=EDGE_CURVE('',#2077,#2077,#1918,.T.);
#2438=EDGE_CURVE('',#2078,#2078,#1919,.T.);
#2439=EDGE_CURVE('',#2078,#2079,#1260,.T.);
#2440=EDGE_CURVE('',#2079,#2079,#1920,.T.);
#2441=EDGE_CURVE('',#2080,#2080,#1921,.T.);
#2442=EDGE_CURVE('',#2080,#2081,#1261,.T.);
#2443=EDGE_CURVE('',#2081,#2081,#1922,.T.);
#2444=EDGE_CURVE('',#2082,#2082,#1923,.T.);
#2445=EDGE_CURVE('',#2082,#2083,#1262,.T.);
#2446=EDGE_CURVE('',#2083,#2083,#1924,.T.);
#2447=EDGE_CURVE('',#2084,#2084,#1925,.T.);
#2448=EDGE_CURVE('',#2084,#2085,#1263,.T.);
#2449=EDGE_CURVE('',#2085,#2085,#1926,.T.);
#2450=EDGE_CURVE('',#2086,#2086,#1927,.T.);
#2451=EDGE_CURVE('',#2086,#2087,#1264,.T.);
#2452=EDGE_CURVE('',#2087,#2087,#1928,.T.);
#2453=EDGE_CURVE('',#2088,#2089,#1265,.T.);
#2454=EDGE_CURVE('',#2089,#2090,#1266,.T.);
#2455=EDGE_CURVE('',#2091,#2090,#1267,.T.);
#2456=EDGE_CURVE('',#2088,#2091,#1268,.T.);
#2457=EDGE_CURVE('',#2092,#2088,#1269,.T.);
#2458=EDGE_CURVE('',#2093,#2091,#1270,.T.);
#2459=EDGE_CURVE('',#2092,#2093,#1271,.T.);
#2460=EDGE_CURVE('',#2094,#2092,#1272,.T.);
#2461=EDGE_CURVE('',#2095,#2093,#1273,.T.);
#2462=EDGE_CURVE('',#2094,#2095,#1274,.T.);
#2463=EDGE_CURVE('',#2089,#2094,#1275,.T.);
#2464=EDGE_CURVE('',#2090,#2095,#1276,.T.);
#2465=EDGE_CURVE('',#2096,#2096,#1929,.T.);
#2466=EDGE_CURVE('',#2096,#2097,#1277,.T.);
#2467=EDGE_CURVE('',#2097,#2097,#1930,.T.);
#2468=EDGE_CURVE('',#2098,#2098,#1931,.T.);
#2469=EDGE_CURVE('',#2098,#2099,#1278,.T.);
#2470=EDGE_CURVE('',#2099,#2099,#1932,.T.);
#2471=EDGE_CURVE('',#2100,#2101,#1279,.T.);
#2472=EDGE_CURVE('',#2101,#2102,#1280,.T.);
#2473=EDGE_CURVE('',#2103,#2102,#1281,.T.);
#2474=EDGE_CURVE('',#2100,#2103,#1282,.T.);
#2475=EDGE_CURVE('',#2104,#2100,#1283,.T.);
#2476=EDGE_CURVE('',#2105,#2103,#1284,.T.);
#2477=EDGE_CURVE('',#2104,#2105,#1285,.T.);
#2478=EDGE_CURVE('',#2106,#2104,#1286,.T.);
#2479=EDGE_CURVE('',#2107,#2105,#1287,.T.);
#2480=EDGE_CURVE('',#2106,#2107,#1288,.T.);
#2481=EDGE_CURVE('',#2101,#2106,#1289,.T.);
#2482=EDGE_CURVE('',#2102,#2107,#1290,.T.);
#2483=EDGE_CURVE('',#2108,#2109,#1291,.T.);
#2484=EDGE_CURVE('',#2109,#2110,#1292,.T.);
#2485=EDGE_CURVE('',#2111,#2110,#1293,.T.);
#2486=EDGE_CURVE('',#2108,#2111,#1294,.T.);
#2487=EDGE_CURVE('',#2112,#2108,#1295,.T.);
#2488=EDGE_CURVE('',#2113,#2111,#1296,.T.);
#2489=EDGE_CURVE('',#2112,#2113,#1297,.T.);
#2490=EDGE_CURVE('',#2114,#2112,#1298,.T.);
#2491=EDGE_CURVE('',#2115,#2113,#1299,.T.);
#2492=EDGE_CURVE('',#2114,#2115,#1300,.T.);
#2493=EDGE_CURVE('',#2109,#2114,#1301,.T.);
#2494=EDGE_CURVE('',#2110,#2115,#1302,.T.);
#2495=EDGE_CURVE('',#2116,#2116,#1933,.T.);
#2496=EDGE_CURVE('',#2116,#2117,#1303,.T.);
#2497=EDGE_CURVE('',#2117,#2117,#1934,.T.);
#2498=EDGE_CURVE('',#2118,#2118,#1935,.T.);
#2499=EDGE_CURVE('',#2118,#2119,#1304,.T.);
#2500=EDGE_CURVE('',#2119,#2119,#1936,.T.);
#2501=EDGE_CURVE('',#2120,#2121,#1305,.T.);
#2502=EDGE_CURVE('',#2121,#2122,#1306,.T.);
#2503=EDGE_CURVE('',#2123,#2122,#1307,.T.);
#2504=EDGE_CURVE('',#2120,#2123,#1308,.T.);
#2505=EDGE_CURVE('',#2124,#2120,#1309,.T.);
#2506=EDGE_CURVE('',#2125,#2123,#1310,.T.);
#2507=EDGE_CURVE('',#2124,#2125,#1311,.T.);
#2508=EDGE_CURVE('',#2126,#2124,#1312,.T.);
#2509=EDGE_CURVE('',#2127,#2125,#1313,.T.);
#2510=EDGE_CURVE('',#2126,#2127,#1314,.T.);
#2511=EDGE_CURVE('',#2121,#2126,#1315,.T.);
#2512=EDGE_CURVE('',#2122,#2127,#1316,.T.);
#2513=EDGE_CURVE('',#2128,#2129,#1317,.T.);
#2514=EDGE_CURVE('',#2129,#2130,#1318,.T.);
#2515=EDGE_CURVE('',#2131,#2130,#1319,.T.);
#2516=EDGE_CURVE('',#2128,#2131,#1320,.T.);
#2517=EDGE_CURVE('',#2132,#2128,#1321,.T.);
#2518=EDGE_CURVE('',#2133,#2131,#1322,.T.);
#2519=EDGE_CURVE('',#2132,#2133,#1323,.T.);
#2520=EDGE_CURVE('',#2134,#2132,#1324,.T.);
#2521=EDGE_CURVE('',#2135,#2133,#1325,.T.);
#2522=EDGE_CURVE('',#2134,#2135,#1326,.T.);
#2523=EDGE_CURVE('',#2129,#2134,#1327,.T.);
#2524=EDGE_CURVE('',#2130,#2135,#1328,.T.);
#2525=EDGE_CURVE('',#2136,#2136,#1937,.T.);
#2526=EDGE_CURVE('',#2136,#2137,#1329,.T.);
#2527=EDGE_CURVE('',#2137,#2137,#1938,.T.);
#2528=EDGE_CURVE('',#2138,#2138,#1939,.T.);
#2529=EDGE_CURVE('',#2138,#2139,#1330,.T.);
#2530=EDGE_CURVE('',#2139,#2139,#1940,.T.);
#2531=EDGE_CURVE('',#2140,#2140,#1941,.T.);
#2532=EDGE_CURVE('',#2140,#2141,#1331,.T.);
#2533=EDGE_CURVE('',#2141,#2141,#1942,.T.);
#2534=EDGE_CURVE('',#2142,#2142,#1943,.T.);
#2535=EDGE_CURVE('',#2142,#2143,#1332,.T.);
#2536=EDGE_CURVE('',#2143,#2143,#1944,.T.);
#2537=EDGE_CURVE('',#2144,#2144,#1945,.T.);
#2538=EDGE_CURVE('',#2144,#2145,#1333,.T.);
#2539=EDGE_CURVE('',#2145,#2145,#1946,.T.);
#2540=EDGE_CURVE('',#2146,#2146,#1947,.T.);
#2541=EDGE_CURVE('',#2146,#2147,#1334,.T.);
#2542=EDGE_CURVE('',#2147,#2147,#1948,.T.);
#2543=EDGE_CURVE('',#2148,#2148,#1949,.T.);
#2544=EDGE_CURVE('',#2148,#2149,#1335,.T.);
#2545=EDGE_CURVE('',#2149,#2149,#1950,.T.);
#2546=EDGE_CURVE('',#2150,#2150,#1951,.T.);
#2547=EDGE_CURVE('',#2150,#2151,#1336,.T.);
#2548=EDGE_CURVE('',#2151,#2151,#1952,.T.);
#2549=EDGE_CURVE('',#2152,#2152,#1953,.T.);
#2550=EDGE_CURVE('',#2152,#2153,#1337,.T.);
#2551=EDGE_CURVE('',#2153,#2153,#1954,.T.);
#2552=EDGE_CURVE('',#2154,#2154,#1955,.T.);
#2553=EDGE_CURVE('',#2154,#2155,#1338,.T.);
#2554=EDGE_CURVE('',#2155,#2155,#1956,.T.);
#2555=EDGE_CURVE('',#2156,#2156,#1957,.T.);
#2556=EDGE_CURVE('',#2156,#2157,#1339,.T.);
#2557=EDGE_CURVE('',#2157,#2157,#1958,.T.);
#2558=EDGE_CURVE('',#2158,#2158,#1959,.T.);
#2559=EDGE_CURVE('',#2158,#2159,#1340,.T.);
#2560=EDGE_CURVE('',#2159,#2159,#1960,.T.);
#2561=EDGE_CURVE('',#2160,#2160,#1961,.T.);
#2562=EDGE_CURVE('',#2160,#2161,#1341,.T.);
#2563=EDGE_CURVE('',#2161,#2161,#1962,.T.);
#2564=EDGE_CURVE('',#2162,#2162,#1963,.T.);
#2565=EDGE_CURVE('',#2162,#2163,#1342,.T.);
#2566=EDGE_CURVE('',#2163,#2163,#1964,.T.);
#2567=EDGE_CURVE('',#2164,#2164,#1965,.T.);
#2568=EDGE_CURVE('',#2165,#2165,#1966,.T.);
#2569=EDGE_CURVE('',#2165,#2164,#1343,.T.);
#2570=EDGE_CURVE('',#2166,#2166,#1967,.T.);
#2571=EDGE_CURVE('',#2166,#2165,#1344,.T.);
#2572=EDGE_CURVE('',#2167,#2167,#1968,.T.);
#2573=EDGE_CURVE('',#2167,#2166,#1345,.T.);
#2574=EDGE_CURVE('',#2168,#2168,#1969,.T.);
#2575=EDGE_CURVE('',#2169,#2169,#1970,.F.);
#2576=EDGE_CURVE('',#2169,#2168,#1346,.T.);
#2577=EDGE_CURVE('',#2170,#2170,#1971,.F.);
#2578=EDGE_CURVE('',#2170,#2169,#1347,.T.);
#2579=EDGE_CURVE('',#2171,#2171,#1972,.T.);
#2580=EDGE_CURVE('',#2171,#2170,#1348,.T.);
#2581=EDGE_CURVE('',#2172,#2173,#1349,.T.);
#2582=EDGE_CURVE('',#2173,#2174,#1350,.T.);
#2583=EDGE_CURVE('',#2174,#2175,#1351,.T.);
#2584=EDGE_CURVE('',#2172,#2175,#1352,.T.);
#2585=EDGE_CURVE('',#2173,#2176,#1353,.T.);
#2586=EDGE_CURVE('',#2176,#2177,#1354,.T.);
#2587=EDGE_CURVE('',#2177,#2174,#1355,.T.);
#2588=EDGE_CURVE('',#2176,#2178,#1356,.T.);
#2589=EDGE_CURVE('',#2178,#2179,#1357,.T.);
#2590=EDGE_CURVE('',#2179,#2177,#1358,.T.);
#2591=EDGE_CURVE('',#2178,#2180,#1359,.T.);
#2592=EDGE_CURVE('',#2180,#2181,#1360,.T.);
#2593=EDGE_CURVE('',#2181,#2179,#1361,.T.);
#2594=EDGE_CURVE('',#2180,#2182,#1362,.T.);
#2595=EDGE_CURVE('',#2182,#2183,#1363,.T.);
#2596=EDGE_CURVE('',#2183,#2181,#1364,.T.);
#2597=EDGE_CURVE('',#2182,#2172,#1365,.T.);
#2598=EDGE_CURVE('',#2175,#2183,#1366,.T.);
#2599=EDGE_CURVE('',#2184,#2184,#1973,.T.);
#2600=EDGE_CURVE('',#2184,#2185,#1367,.T.);
#2601=EDGE_CURVE('',#2185,#2185,#1974,.T.);
#2602=EDGE_CURVE('',#2186,#2186,#1975,.T.);
#2603=EDGE_CURVE('',#2186,#2187,#1368,.T.);
#2604=EDGE_CURVE('',#2187,#2187,#1976,.T.);
#2605=EDGE_CURVE('',#2188,#2189,#1977,.T.);
#2606=EDGE_CURVE('',#2190,#2191,#1369,.T.);
#2607=EDGE_CURVE('',#2190,#2192,#1370,.T.);
#2608=EDGE_CURVE('',#2191,#2192,#1978,.T.);
#2609=EDGE_CURVE('',#2193,#2194,#1371,.T.);
#2610=EDGE_CURVE('',#2195,#2193,#1979,.T.);
#2611=EDGE_CURVE('',#2195,#2194,#1372,.T.);
#2612=EDGE_CURVE('',#2196,#2197,#1373,.T.);
#2613=EDGE_CURVE('',#2198,#2196,#1980,.T.);
#2614=EDGE_CURVE('',#2198,#2197,#1374,.T.);
#2615=EDGE_CURVE('',#2197,#2190,#1375,.T.);
#2616=EDGE_CURVE('',#2192,#2198,#1376,.T.);
#2617=EDGE_CURVE('',#2199,#2200,#1377,.T.);
#2618=EDGE_CURVE('',#2199,#2201,#1378,.T.);
#2619=EDGE_CURVE('',#2200,#2201,#1981,.T.);
#2620=EDGE_CURVE('',#2194,#2199,#1379,.T.);
#2621=EDGE_CURVE('',#2201,#2195,#1380,.T.);
#2622=EDGE_CURVE('',#2202,#2203,#1381,.T.);
#2623=EDGE_CURVE('',#2203,#2204,#1382,.T.);
#2624=EDGE_CURVE('',#2204,#2205,#1383,.T.);
#2625=EDGE_CURVE('',#2205,#2202,#1384,.T.);
#2626=EDGE_CURVE('',#2206,#2206,#1982,.T.);
#2627=EDGE_CURVE('',#2207,#2207,#1983,.T.);
#2628=EDGE_CURVE('',#2200,#2208,#1385,.T.);
#2629=EDGE_CURVE('',#2208,#2209,#1386,.T.);
#2630=EDGE_CURVE('',#2209,#2196,#1387,.T.);
#2631=EDGE_CURVE('',#2191,#2210,#1388,.T.);
#2632=EDGE_CURVE('',#2210,#2211,#1389,.T.);
#2633=EDGE_CURVE('',#2211,#2193,#1390,.T.);
#2634=EDGE_CURVE('',#2210,#2211,#1984,.T.);
#2635=EDGE_CURVE('',#2208,#2209,#1985,.T.);
#2636=EDGE_CURVE('',#2212,#2213,#1391,.T.);
#2637=EDGE_CURVE('',#2212,#2214,#1392,.T.);
#2638=EDGE_CURVE('',#2214,#2215,#1393,.T.);
#2639=EDGE_CURVE('',#2213,#2215,#1394,.T.);
#2640=EDGE_CURVE('',#2216,#2212,#1395,.T.);
#2641=EDGE_CURVE('',#2216,#2217,#1396,.T.);
#2642=EDGE_CURVE('',#2217,#2214,#1397,.T.);
#2643=EDGE_CURVE('',#2218,#2216,#1398,.T.);
#2644=EDGE_CURVE('',#2218,#2219,#1399,.T.);
#2645=EDGE_CURVE('',#2219,#2217,#1400,.T.);
#2646=EDGE_CURVE('',#2213,#2218,#1401,.T.);
#2647=EDGE_CURVE('',#2215,#2219,#1402,.T.);
#2648=EDGE_CURVE('',#2220,#2220,#1986,.T.);
#2649=EDGE_CURVE('',#2220,#2207,#1403,.T.);
#2650=EDGE_CURVE('',#2221,#2221,#1987,.T.);
#2651=EDGE_CURVE('',#2221,#2206,#1404,.T.);
#2652=EDGE_CURVE('',#2222,#2223,#1405,.T.);
#2653=EDGE_CURVE('',#2223,#2202,#1406,.T.);
#2654=EDGE_CURVE('',#2222,#2205,#1407,.T.);
#2655=EDGE_CURVE('',#2224,#2222,#1408,.T.);
#2656=EDGE_CURVE('',#2224,#2204,#1409,.T.);
#2657=EDGE_CURVE('',#2225,#2224,#1410,.T.);
#2658=EDGE_CURVE('',#2225,#2203,#1411,.T.);
#2659=EDGE_CURVE('',#2223,#2225,#1412,.T.);
#2660=EDGE_CURVE('',#2226,#2226,#1988,.T.);
#2661=EDGE_CURVE('',#2226,#2227,#1413,.T.);
#2662=EDGE_CURVE('',#2227,#2227,#1989,.T.);
#2663=EDGE_CURVE('',#2228,#2228,#1990,.T.);
#2664=EDGE_CURVE('',#2229,#2230,#1991,.T.);
#2665=EDGE_CURVE('',#2231,#2231,#1992,.T.);
#2666=EDGE_CURVE('',#2232,#2233,#223,.T.);
#2667=EDGE_CURVE('',#2234,#2232,#224,.T.);
#2668=EDGE_CURVE('',#2233,#2234,#225,.T.);
#2669=EDGE_CURVE('',#2233,#2235,#1414,.T.);
#2670=EDGE_CURVE('',#2235,#2235,#226,.T.);
#2671=EDGE_CURVE('',#2236,#2236,#227,.T.);
#2672=EDGE_CURVE('',#2236,#2237,#1415,.T.);
#2673=EDGE_CURVE('',#2238,#2237,#228,.T.);
#2674=EDGE_CURVE('',#2239,#2238,#229,.T.);
#2675=EDGE_CURVE('',#2237,#2239,#230,.T.);
#2676=EDGE_CURVE('',#2240,#2240,#1993,.T.);
#2677=EDGE_CURVE('',#2240,#2241,#1416,.T.);
#2678=EDGE_CURVE('',#2241,#2241,#1994,.T.);
#2679=EDGE_CURVE('',#2242,#2243,#231,.T.);
#2680=EDGE_CURVE('',#2243,#2244,#232,.T.);
#2681=EDGE_CURVE('',#2244,#2242,#233,.T.);
#2682=EDGE_CURVE('',#2245,#2246,#234,.T.);
#2683=EDGE_CURVE('',#2246,#2247,#235,.T.);
#2684=EDGE_CURVE('',#2247,#2245,#236,.T.);
#2685=EDGE_CURVE('',#2248,#2249,#237,.T.);
#2686=EDGE_CURVE('',#2249,#2250,#238,.T.);
#2687=EDGE_CURVE('',#2250,#2248,#239,.T.);
#2688=EDGE_CURVE('',#2251,#2252,#240,.T.);
#2689=EDGE_CURVE('',#2252,#2253,#241,.T.);
#2690=EDGE_CURVE('',#2253,#2251,#242,.T.);
#2691=EDGE_CURVE('',#2244,#2254,#1417,.T.);
#2692=EDGE_CURVE('',#2254,#2254,#243,.T.);
#2693=EDGE_CURVE('',#2255,#2255,#244,.T.);
#2694=EDGE_CURVE('',#2255,#2247,#1418,.T.);
#2695=EDGE_CURVE('',#2250,#2256,#1419,.T.);
#2696=EDGE_CURVE('',#2256,#2256,#245,.T.);
#2697=EDGE_CURVE('',#2257,#2257,#246,.T.);
#2698=EDGE_CURVE('',#2257,#2253,#1420,.T.);
#2699=EDGE_CURVE('',#2258,#2258,#1995,.T.);
#2700=EDGE_CURVE('',#2259,#2259,#1996,.T.);
#2701=EDGE_CURVE('',#2260,#2260,#1997,.T.);
#2702=EDGE_CURVE('',#2260,#2259,#1421,.T.);
#2703=EDGE_CURVE('',#2261,#2261,#1998,.T.);
#2704=EDGE_CURVE('',#2261,#2258,#1422,.T.);
#2705=EDGE_CURVE('',#2262,#2262,#1999,.T.);
#2706=EDGE_CURVE('',#2262,#2263,#1423,.T.);
#2707=EDGE_CURVE('',#2263,#2263,#2000,.T.);
#2708=EDGE_CURVE('',#2264,#2264,#2001,.T.);
#2709=EDGE_CURVE('',#2264,#2265,#1424,.T.);
#2710=EDGE_CURVE('',#2265,#2265,#2002,.T.);
#2711=EDGE_CURVE('',#2266,#2267,#1425,.T.);
#2712=EDGE_CURVE('',#2267,#2268,#1426,.T.);
#2713=EDGE_CURVE('',#2268,#2269,#1427,.T.);
#2714=EDGE_CURVE('',#2266,#2269,#1428,.T.);
#2715=EDGE_CURVE('',#2267,#2270,#1429,.T.);
#2716=EDGE_CURVE('',#2270,#2271,#1430,.T.);
#2717=EDGE_CURVE('',#2271,#2268,#1431,.T.);
#2718=EDGE_CURVE('',#2270,#2272,#1432,.T.);
#2719=EDGE_CURVE('',#2272,#2273,#1433,.T.);
#2720=EDGE_CURVE('',#2273,#2271,#1434,.T.);
#2721=EDGE_CURVE('',#2272,#2274,#1435,.T.);
#2722=EDGE_CURVE('',#2274,#2275,#1436,.T.);
#2723=EDGE_CURVE('',#2275,#2273,#1437,.T.);
#2724=EDGE_CURVE('',#2274,#2276,#1438,.T.);
#2725=EDGE_CURVE('',#2276,#2277,#1439,.T.);
#2726=EDGE_CURVE('',#2277,#2275,#1440,.T.);
#2727=EDGE_CURVE('',#2276,#2266,#1441,.T.);
#2728=EDGE_CURVE('',#2269,#2277,#1442,.T.);
#2729=EDGE_CURVE('',#2278,#2278,#2003,.T.);
#2730=EDGE_CURVE('',#2279,#2279,#2004,.T.);
#2731=EDGE_CURVE('',#2280,#2280,#2005,.T.);
#2732=EDGE_CURVE('',#2280,#2279,#1443,.T.);
#2733=EDGE_CURVE('',#2281,#2281,#2006,.T.);
#2734=EDGE_CURVE('',#2281,#2280,#1444,.T.);
#2735=EDGE_CURVE('',#2282,#2282,#2007,.T.);
#2736=EDGE_CURVE('',#2282,#2281,#1445,.T.);
#2737=EDGE_CURVE('',#2283,#2283,#2008,.T.);
#2738=EDGE_CURVE('',#2284,#2284,#2009,.F.);
#2739=EDGE_CURVE('',#2284,#2283,#1446,.T.);
#2740=EDGE_CURVE('',#2278,#2284,#1447,.T.);
#2741=EDGE_CURVE('',#2285,#2285,#2010,.T.);
#2742=EDGE_CURVE('',#2285,#2286,#1448,.T.);
#2743=EDGE_CURVE('',#2286,#2286,#2011,.T.);
#2744=EDGE_CURVE('',#2287,#2287,#2012,.T.);
#2745=EDGE_CURVE('',#2287,#2288,#1449,.T.);
#2746=EDGE_CURVE('',#2288,#2288,#2013,.T.);
#2747=EDGE_CURVE('',#2289,#2290,#1450,.T.);
#2748=EDGE_CURVE('',#2289,#2291,#1451,.T.);
#2749=EDGE_CURVE('',#2292,#2291,#1452,.T.);
#2750=EDGE_CURVE('',#2292,#2290,#1453,.T.);
#2751=EDGE_CURVE('',#2290,#2293,#2014,.T.);
#2752=EDGE_CURVE('',#2294,#2292,#1454,.T.);
#2753=EDGE_CURVE('',#2293,#2294,#1455,.T.);
#2754=EDGE_CURVE('',#2293,#2295,#1456,.T.);
#2755=EDGE_CURVE('',#2294,#2296,#1457,.T.);
#2756=EDGE_CURVE('',#2296,#2295,#1458,.T.);
#2757=EDGE_CURVE('',#2291,#2296,#1459,.T.);
#2758=EDGE_CURVE('',#2295,#2289,#2015,.T.);
#2759=EDGE_CURVE('',#2297,#2298,#1460,.T.);
#2760=EDGE_CURVE('',#2297,#2299,#1461,.T.);
#2761=EDGE_CURVE('',#2300,#2299,#1462,.T.);
#2762=EDGE_CURVE('',#2300,#2298,#1463,.T.);
#2763=EDGE_CURVE('',#2298,#2301,#2016,.T.);
#2764=EDGE_CURVE('',#2302,#2300,#1464,.T.);
#2765=EDGE_CURVE('',#2301,#2302,#1465,.T.);
#2766=EDGE_CURVE('',#2301,#2303,#1466,.T.);
#2767=EDGE_CURVE('',#2302,#2304,#1467,.T.);
#2768=EDGE_CURVE('',#2304,#2303,#1468,.T.);
#2769=EDGE_CURVE('',#2299,#2304,#1469,.T.);
#2770=EDGE_CURVE('',#2303,#2297,#2017,.T.);
#2771=EDGE_CURVE('',#2305,#2305,#2018,.T.);
#2772=EDGE_CURVE('',#2305,#2306,#1470,.T.);
#2773=EDGE_CURVE('',#2306,#2306,#2019,.T.);
#2774=EDGE_CURVE('',#2307,#2308,#1471,.T.);
#2775=EDGE_CURVE('',#2307,#2308,#2020,.T.);
#2776=EDGE_CURVE('',#2309,#2307,#247,.T.);
#2777=EDGE_CURVE('',#2310,#2309,#2021,.T.);
#2778=EDGE_CURVE('',#2310,#2311,#1472,.T.);
#2779=EDGE_CURVE('',#2312,#2311,#248,.T.);
#2780=EDGE_CURVE('',#2311,#2312,#249,.T.);
#2781=EDGE_CURVE('',#2313,#2310,#2022,.T.);
#2782=EDGE_CURVE('',#2308,#2313,#250,.T.);
#2783=EDGE_CURVE('',#2313,#2309,#1473,.T.);
#2784=EDGE_CURVE('',#2314,#2315,#1474,.T.);
#2785=EDGE_CURVE('',#2314,#2316,#1475,.T.);
#2786=EDGE_CURVE('',#2317,#2316,#1476,.T.);
#2787=EDGE_CURVE('',#2315,#2317,#1477,.T.);
#2788=EDGE_CURVE('',#2318,#2314,#1478,.T.);
#2789=EDGE_CURVE('',#2318,#2319,#1479,.T.);
#2790=EDGE_CURVE('',#2316,#2319,#1480,.T.);
#2791=EDGE_CURVE('',#2320,#2318,#1481,.T.);
#2792=EDGE_CURVE('',#2321,#2320,#1482,.T.);
#2793=EDGE_CURVE('',#2319,#2321,#1483,.T.);
#2794=EDGE_CURVE('',#2322,#2322,#2023,.T.);
#2795=EDGE_CURVE('',#2321,#2317,#2024,.T.);
#2796=EDGE_CURVE('',#2320,#2315,#2025,.T.);
#2797=EDGE_CURVE('',#2322,#2323,#1484,.T.);
#2798=EDGE_CURVE('',#2323,#2323,#2026,.T.);
#2799=EDGE_CURVE('',#2324,#2325,#1485,.T.);
#2800=EDGE_CURVE('',#2324,#2325,#2027,.T.);
#2801=EDGE_CURVE('',#2326,#2324,#251,.T.);
#2802=EDGE_CURVE('',#2327,#2326,#2028,.T.);
#2803=EDGE_CURVE('',#2327,#2328,#1486,.T.);
#2804=EDGE_CURVE('',#2329,#2328,#252,.T.);
#2805=EDGE_CURVE('',#2328,#2329,#253,.T.);
#2806=EDGE_CURVE('',#2330,#2327,#2029,.T.);
#2807=EDGE_CURVE('',#2325,#2330,#254,.T.);
#2808=EDGE_CURVE('',#2330,#2326,#1487,.T.);
#2809=EDGE_CURVE('',#2331,#2332,#1488,.T.);
#2810=EDGE_CURVE('',#2331,#2333,#1489,.T.);
#2811=EDGE_CURVE('',#2334,#2333,#1490,.T.);
#2812=EDGE_CURVE('',#2332,#2334,#1491,.T.);
#2813=EDGE_CURVE('',#2335,#2331,#1492,.T.);
#2814=EDGE_CURVE('',#2335,#2336,#1493,.T.);
#2815=EDGE_CURVE('',#2333,#2336,#1494,.T.);
#2816=EDGE_CURVE('',#2337,#2335,#1495,.T.);
#2817=EDGE_CURVE('',#2338,#2337,#1496,.T.);
#2818=EDGE_CURVE('',#2336,#2338,#1497,.T.);
#2819=EDGE_CURVE('',#2339,#2339,#2030,.T.);
#2820=EDGE_CURVE('',#2338,#2334,#2031,.T.);
#2821=EDGE_CURVE('',#2337,#2332,#2032,.T.);
#2822=EDGE_CURVE('',#2339,#2340,#1498,.T.);
#2823=EDGE_CURVE('',#2340,#2340,#2033,.T.);
#2824=EDGE_CURVE('',#2341,#2342,#1499,.T.);
#2825=EDGE_CURVE('',#2341,#2342,#2034,.T.);
#2826=EDGE_CURVE('',#2343,#2341,#255,.T.);
#2827=EDGE_CURVE('',#2344,#2343,#2035,.T.);
#2828=EDGE_CURVE('',#2344,#2345,#1500,.T.);
#2829=EDGE_CURVE('',#2346,#2345,#256,.T.);
#2830=EDGE_CURVE('',#2345,#2346,#257,.T.);
#2831=EDGE_CURVE('',#2347,#2344,#2036,.T.);
#2832=EDGE_CURVE('',#2342,#2347,#258,.T.);
#2833=EDGE_CURVE('',#2347,#2343,#1501,.T.);
#2834=EDGE_CURVE('',#2348,#2348,#2037,.T.);
#2835=EDGE_CURVE('',#2348,#2349,#1502,.T.);
#2836=EDGE_CURVE('',#2349,#2349,#2038,.T.);
#2837=EDGE_CURVE('',#2350,#2350,#2039,.T.);
#2838=EDGE_CURVE('',#2350,#2351,#1503,.T.);
#2839=EDGE_CURVE('',#2351,#2351,#2040,.T.);
#2840=EDGE_CURVE('',#2352,#2353,#1504,.T.);
#2841=EDGE_CURVE('',#2352,#2353,#2041,.T.);
#2842=EDGE_CURVE('',#2354,#2352,#259,.T.);
#2843=EDGE_CURVE('',#2355,#2354,#2042,.T.);
#2844=EDGE_CURVE('',#2355,#2356,#1505,.T.);
#2845=EDGE_CURVE('',#2357,#2356,#260,.T.);
#2846=EDGE_CURVE('',#2356,#2357,#261,.T.);
#2847=EDGE_CURVE('',#2358,#2355,#2043,.T.);
#2848=EDGE_CURVE('',#2353,#2358,#262,.T.);
#2849=EDGE_CURVE('',#2358,#2354,#1506,.T.);
#2850=EDGE_CURVE('',#2359,#2359,#2044,.T.);
#2851=EDGE_CURVE('',#2359,#2360,#1507,.T.);
#2852=EDGE_CURVE('',#2360,#2360,#2045,.T.);
#2853=EDGE_CURVE('',#2361,#2361,#2046,.T.);
#2854=EDGE_CURVE('',#2361,#2362,#1508,.T.);
#2855=EDGE_CURVE('',#2362,#2362,#2047,.T.);
#2856=EDGE_CURVE('',#2363,#2363,#2048,.T.);
#2857=EDGE_CURVE('',#2363,#2364,#1509,.T.);
#2858=EDGE_CURVE('',#2364,#2364,#2049,.T.);
#2859=EDGE_CURVE('',#2365,#2365,#2050,.T.);
#2860=EDGE_CURVE('',#2365,#2366,#1510,.T.);
#2861=EDGE_CURVE('',#2366,#2366,#2051,.T.);
#2862=EDGE_CURVE('',#2367,#2367,#2052,.T.);
#2863=EDGE_CURVE('',#2367,#2368,#1511,.T.);
#2864=EDGE_CURVE('',#2368,#2368,#2053,.T.);
#2865=EDGE_CURVE('',#2369,#2369,#2054,.T.);
#2866=EDGE_CURVE('',#2369,#2370,#1512,.T.);
#2867=EDGE_CURVE('',#2370,#2370,#2055,.T.);
#2868=EDGE_CURVE('',#2371,#2372,#1513,.T.);
#2869=EDGE_CURVE('',#2373,#2371,#1514,.T.);
#2870=EDGE_CURVE('',#2374,#2373,#1515,.T.);
#2871=EDGE_CURVE('',#2375,#2374,#1516,.T.);
#2872=EDGE_CURVE('',#2376,#2375,#1517,.T.);
#2873=EDGE_CURVE('',#2377,#2376,#1518,.T.);
#2874=EDGE_CURVE('',#2378,#2377,#1519,.T.);
#2875=EDGE_CURVE('',#2372,#2378,#1520,.T.);
#2876=EDGE_CURVE('',#2375,#2379,#1521,.T.);
#2877=EDGE_CURVE('',#2379,#2380,#1522,.T.);
#2878=EDGE_CURVE('',#2380,#2376,#1523,.T.);
#2879=EDGE_CURVE('',#2381,#2374,#1524,.T.);
#2880=EDGE_CURVE('',#2381,#2379,#1525,.T.);
#2881=EDGE_CURVE('',#2373,#2382,#1526,.T.);
#2882=EDGE_CURVE('',#2382,#2381,#1527,.T.);
#2883=EDGE_CURVE('',#2383,#2371,#1528,.T.);
#2884=EDGE_CURVE('',#2383,#2382,#1529,.T.);
#2885=EDGE_CURVE('',#2384,#2385,#1530,.T.);
#2886=EDGE_CURVE('',#2380,#2384,#1531,.T.);
#2887=EDGE_CURVE('',#2386,#2383,#1532,.T.);
#2888=EDGE_CURVE('',#2385,#2386,#1533,.T.);
#2889=EDGE_CURVE('',#2377,#2384,#1534,.T.);
#2890=EDGE_CURVE('',#2372,#2386,#1535,.T.);
#2891=EDGE_CURVE('',#2385,#2378,#1536,.T.);
#2892=EDGE_CURVE('',#2387,#2388,#1537,.T.);
#2893=EDGE_CURVE('',#2387,#2389,#1538,.T.);
#2894=EDGE_CURVE('',#2389,#2390,#1539,.T.);
#2895=EDGE_CURVE('',#2388,#2390,#1540,.T.);
#2896=EDGE_CURVE('',#2391,#2387,#1541,.T.);
#2897=EDGE_CURVE('',#2391,#2392,#1542,.T.);
#2898=EDGE_CURVE('',#2392,#2389,#1543,.T.);
#2899=EDGE_CURVE('',#2393,#2391,#1544,.T.);
#2900=EDGE_CURVE('',#2393,#2394,#1545,.T.);
#2901=EDGE_CURVE('',#2394,#2392,#1546,.T.);
#2902=EDGE_CURVE('',#2395,#2393,#1547,.T.);
#2903=EDGE_CURVE('',#2395,#2396,#1548,.T.);
#2904=EDGE_CURVE('',#2396,#2394,#1549,.T.);
#2905=EDGE_CURVE('',#2397,#2395,#1550,.T.);
#2906=EDGE_CURVE('',#2397,#2398,#1551,.T.);
#2907=EDGE_CURVE('',#2398,#2396,#1552,.T.);
#2908=EDGE_CURVE('',#2388,#2397,#1553,.T.);
#2909=EDGE_CURVE('',#2390,#2398,#1554,.T.);
#2910=EDGE_CURVE('',#2399,#2399,#2056,.T.);
#2911=EDGE_CURVE('',#2400,#2400,#2057,.T.);
#2912=EDGE_CURVE('',#2400,#2399,#1555,.T.);
#2913=EDGE_CURVE('',#2401,#2401,#2058,.F.);
#2914=EDGE_CURVE('',#2401,#2400,#1556,.T.);
#2915=EDGE_CURVE('',#2402,#2402,#2059,.T.);
#2916=EDGE_CURVE('',#2402,#2401,#1557,.T.);
#2917=EDGE_CURVE('',#2403,#2403,#2060,.T.);
#2918=EDGE_CURVE('',#2404,#2404,#2061,.T.);
#2919=EDGE_CURVE('',#2404,#2403,#1558,.T.);
#2920=EDGE_CURVE('',#2405,#2405,#2062,.T.);
#2921=EDGE_CURVE('',#2405,#2404,#1559,.T.);
#2922=EDGE_CURVE('',#2406,#2406,#2063,.T.);
#2923=EDGE_CURVE('',#2406,#2405,#1560,.T.);
#2924=EDGE_CURVE('',#2407,#2407,#2064,.T.);
#2925=EDGE_CURVE('',#2408,#2408,#2065,.F.);
#2926=EDGE_CURVE('',#2408,#2407,#1561,.T.);
#2927=EDGE_CURVE('',#2409,#2409,#2066,.F.);
#2928=EDGE_CURVE('',#2409,#2408,#1562,.T.);
#2929=EDGE_CURVE('',#2410,#2410,#2067,.T.);
#2930=EDGE_CURVE('',#2410,#2409,#1563,.T.);
#2931=EDGE_CURVE('',#2411,#2412,#1564,.T.);
#2932=EDGE_CURVE('',#2412,#2413,#1565,.T.);
#2933=EDGE_CURVE('',#2413,#2414,#1566,.T.);
#2934=EDGE_CURVE('',#2411,#2414,#1567,.T.);
#2935=EDGE_CURVE('',#2412,#2415,#1568,.T.);
#2936=EDGE_CURVE('',#2415,#2416,#1569,.T.);
#2937=EDGE_CURVE('',#2416,#2413,#1570,.T.);
#2938=EDGE_CURVE('',#2415,#2417,#1571,.T.);
#2939=EDGE_CURVE('',#2417,#2418,#1572,.T.);
#2940=EDGE_CURVE('',#2418,#2416,#1573,.T.);
#2941=EDGE_CURVE('',#2417,#2419,#1574,.T.);
#2942=EDGE_CURVE('',#2419,#2420,#1575,.T.);
#2943=EDGE_CURVE('',#2420,#2418,#1576,.T.);
#2944=EDGE_CURVE('',#2419,#2421,#1577,.T.);
#2945=EDGE_CURVE('',#2421,#2422,#1578,.T.);
#2946=EDGE_CURVE('',#2422,#2420,#1579,.T.);
#2947=EDGE_CURVE('',#2421,#2411,#1580,.T.);
#2948=EDGE_CURVE('',#2414,#2422,#1581,.T.);
#2949=ORIENTED_EDGE('',*,*,#2423,.F.);
#2950=ORIENTED_EDGE('',*,*,#2424,.T.);
#2951=ORIENTED_EDGE('',*,*,#2425,.F.);
#2952=ORIENTED_EDGE('',*,*,#2424,.F.);
#2953=ORIENTED_EDGE('',*,*,#2426,.F.);
#2954=ORIENTED_EDGE('',*,*,#2427,.T.);
#2955=ORIENTED_EDGE('',*,*,#2428,.F.);
#2956=ORIENTED_EDGE('',*,*,#2427,.F.);
#2957=ORIENTED_EDGE('',*,*,#2429,.F.);
#2958=ORIENTED_EDGE('',*,*,#2430,.T.);
#2959=ORIENTED_EDGE('',*,*,#2431,.F.);
#2960=ORIENTED_EDGE('',*,*,#2430,.F.);
#2961=ORIENTED_EDGE('',*,*,#2432,.F.);
#2962=ORIENTED_EDGE('',*,*,#2433,.T.);
#2963=ORIENTED_EDGE('',*,*,#2434,.F.);
#2964=ORIENTED_EDGE('',*,*,#2433,.F.);
#2965=ORIENTED_EDGE('',*,*,#2435,.F.);
#2966=ORIENTED_EDGE('',*,*,#2436,.T.);
#2967=ORIENTED_EDGE('',*,*,#2437,.F.);
#2968=ORIENTED_EDGE('',*,*,#2436,.F.);
#2969=ORIENTED_EDGE('',*,*,#2438,.F.);
#2970=ORIENTED_EDGE('',*,*,#2439,.T.);
#2971=ORIENTED_EDGE('',*,*,#2440,.F.);
#2972=ORIENTED_EDGE('',*,*,#2439,.F.);
#2973=ORIENTED_EDGE('',*,*,#2441,.F.);
#2974=ORIENTED_EDGE('',*,*,#2442,.T.);
#2975=ORIENTED_EDGE('',*,*,#2443,.F.);
#2976=ORIENTED_EDGE('',*,*,#2442,.F.);
#2977=ORIENTED_EDGE('',*,*,#2444,.F.);
#2978=ORIENTED_EDGE('',*,*,#2445,.T.);
#2979=ORIENTED_EDGE('',*,*,#2446,.F.);
#2980=ORIENTED_EDGE('',*,*,#2445,.F.);
#2981=ORIENTED_EDGE('',*,*,#2447,.F.);
#2982=ORIENTED_EDGE('',*,*,#2448,.T.);
#2983=ORIENTED_EDGE('',*,*,#2449,.F.);
#2984=ORIENTED_EDGE('',*,*,#2448,.F.);
#2985=ORIENTED_EDGE('',*,*,#2450,.F.);
#2986=ORIENTED_EDGE('',*,*,#2451,.T.);
#2987=ORIENTED_EDGE('',*,*,#2452,.F.);
#2988=ORIENTED_EDGE('',*,*,#2451,.F.);
#2989=ORIENTED_EDGE('',*,*,#2453,.T.);
#2990=ORIENTED_EDGE('',*,*,#2454,.T.);
#2991=ORIENTED_EDGE('',*,*,#2455,.F.);
#2992=ORIENTED_EDGE('',*,*,#2456,.F.);
#2993=ORIENTED_EDGE('',*,*,#2457,.T.);
#2994=ORIENTED_EDGE('',*,*,#2456,.T.);
#2995=ORIENTED_EDGE('',*,*,#2458,.F.);
#2996=ORIENTED_EDGE('',*,*,#2459,.F.);
#2997=ORIENTED_EDGE('',*,*,#2460,.T.);
#2998=ORIENTED_EDGE('',*,*,#2459,.T.);
#2999=ORIENTED_EDGE('',*,*,#2461,.F.);
#3000=ORIENTED_EDGE('',*,*,#2462,.F.);
#3001=ORIENTED_EDGE('',*,*,#2463,.T.);
#3002=ORIENTED_EDGE('',*,*,#2462,.T.);
#3003=ORIENTED_EDGE('',*,*,#2464,.F.);
#3004=ORIENTED_EDGE('',*,*,#2454,.F.);
#3005=ORIENTED_EDGE('',*,*,#2464,.T.);
#3006=ORIENTED_EDGE('',*,*,#2461,.T.);
#3007=ORIENTED_EDGE('',*,*,#2458,.T.);
#3008=ORIENTED_EDGE('',*,*,#2455,.T.);
#3009=ORIENTED_EDGE('',*,*,#2437,.T.);
#3010=ORIENTED_EDGE('',*,*,#2440,.T.);
#3011=ORIENTED_EDGE('',*,*,#2443,.T.);
#3012=ORIENTED_EDGE('',*,*,#2446,.T.);
#3013=ORIENTED_EDGE('',*,*,#2449,.T.);
#3014=ORIENTED_EDGE('',*,*,#2452,.T.);
#3015=ORIENTED_EDGE('',*,*,#2434,.T.);
#3016=ORIENTED_EDGE('',*,*,#2431,.T.);
#3017=ORIENTED_EDGE('',*,*,#2428,.T.);
#3018=ORIENTED_EDGE('',*,*,#2425,.T.);
#3019=ORIENTED_EDGE('',*,*,#2463,.F.);
#3020=ORIENTED_EDGE('',*,*,#2453,.F.);
#3021=ORIENTED_EDGE('',*,*,#2457,.F.);
#3022=ORIENTED_EDGE('',*,*,#2460,.F.);
#3023=ORIENTED_EDGE('',*,*,#2435,.T.);
#3024=ORIENTED_EDGE('',*,*,#2438,.T.);
#3025=ORIENTED_EDGE('',*,*,#2441,.T.);
#3026=ORIENTED_EDGE('',*,*,#2444,.T.);
#3027=ORIENTED_EDGE('',*,*,#2447,.T.);
#3028=ORIENTED_EDGE('',*,*,#2450,.T.);
#3029=ORIENTED_EDGE('',*,*,#2432,.T.);
#3030=ORIENTED_EDGE('',*,*,#2429,.T.);
#3031=ORIENTED_EDGE('',*,*,#2426,.T.);
#3032=ORIENTED_EDGE('',*,*,#2423,.T.);
#3033=ORIENTED_EDGE('',*,*,#2465,.F.);
#3034=ORIENTED_EDGE('',*,*,#2466,.T.);
#3035=ORIENTED_EDGE('',*,*,#2467,.F.);
#3036=ORIENTED_EDGE('',*,*,#2466,.F.);
#3037=ORIENTED_EDGE('',*,*,#2465,.T.);
#3038=ORIENTED_EDGE('',*,*,#2468,.F.);
#3039=ORIENTED_EDGE('',*,*,#2469,.T.);
#3040=ORIENTED_EDGE('',*,*,#2470,.F.);
#3041=ORIENTED_EDGE('',*,*,#2469,.F.);
#3042=ORIENTED_EDGE('',*,*,#2468,.T.);
#3043=ORIENTED_EDGE('',*,*,#2471,.T.);
#3044=ORIENTED_EDGE('',*,*,#2472,.T.);
#3045=ORIENTED_EDGE('',*,*,#2473,.F.);
#3046=ORIENTED_EDGE('',*,*,#2474,.F.);
#3047=ORIENTED_EDGE('',*,*,#2475,.T.);
#3048=ORIENTED_EDGE('',*,*,#2474,.T.);
#3049=ORIENTED_EDGE('',*,*,#2476,.F.);
#3050=ORIENTED_EDGE('',*,*,#2477,.F.);
#3051=ORIENTED_EDGE('',*,*,#2478,.T.);
#3052=ORIENTED_EDGE('',*,*,#2477,.T.);
#3053=ORIENTED_EDGE('',*,*,#2479,.F.);
#3054=ORIENTED_EDGE('',*,*,#2480,.F.);
#3055=ORIENTED_EDGE('',*,*,#2481,.T.);
#3056=ORIENTED_EDGE('',*,*,#2480,.T.);
#3057=ORIENTED_EDGE('',*,*,#2482,.F.);
#3058=ORIENTED_EDGE('',*,*,#2472,.F.);
#3059=ORIENTED_EDGE('',*,*,#2482,.T.);
#3060=ORIENTED_EDGE('',*,*,#2479,.T.);
#3061=ORIENTED_EDGE('',*,*,#2476,.T.);
#3062=ORIENTED_EDGE('',*,*,#2473,.T.);
#3063=ORIENTED_EDGE('',*,*,#2467,.T.);
#3064=ORIENTED_EDGE('',*,*,#2470,.T.);
#3065=ORIENTED_EDGE('',*,*,#2481,.F.);
#3066=ORIENTED_EDGE('',*,*,#2471,.F.);
#3067=ORIENTED_EDGE('',*,*,#2475,.F.);
#3068=ORIENTED_EDGE('',*,*,#2478,.F.);
#3069=ORIENTED_EDGE('',*,*,#2483,.T.);
#3070=ORIENTED_EDGE('',*,*,#2484,.T.);
#3071=ORIENTED_EDGE('',*,*,#2485,.F.);
#3072=ORIENTED_EDGE('',*,*,#2486,.F.);
#3073=ORIENTED_EDGE('',*,*,#2487,.T.);
#3074=ORIENTED_EDGE('',*,*,#2486,.T.);
#3075=ORIENTED_EDGE('',*,*,#2488,.F.);
#3076=ORIENTED_EDGE('',*,*,#2489,.F.);
#3077=ORIENTED_EDGE('',*,*,#2490,.T.);
#3078=ORIENTED_EDGE('',*,*,#2489,.T.);
#3079=ORIENTED_EDGE('',*,*,#2491,.F.);
#3080=ORIENTED_EDGE('',*,*,#2492,.F.);
#3081=ORIENTED_EDGE('',*,*,#2493,.T.);
#3082=ORIENTED_EDGE('',*,*,#2492,.T.);
#3083=ORIENTED_EDGE('',*,*,#2494,.F.);
#3084=ORIENTED_EDGE('',*,*,#2484,.F.);
#3085=ORIENTED_EDGE('',*,*,#2494,.T.);
#3086=ORIENTED_EDGE('',*,*,#2491,.T.);
#3087=ORIENTED_EDGE('',*,*,#2488,.T.);
#3088=ORIENTED_EDGE('',*,*,#2485,.T.);
#3089=ORIENTED_EDGE('',*,*,#2493,.F.);
#3090=ORIENTED_EDGE('',*,*,#2483,.F.);
#3091=ORIENTED_EDGE('',*,*,#2487,.F.);
#3092=ORIENTED_EDGE('',*,*,#2490,.F.);
#3093=ORIENTED_EDGE('',*,*,#2495,.F.);
#3094=ORIENTED_EDGE('',*,*,#2496,.T.);
#3095=ORIENTED_EDGE('',*,*,#2497,.F.);
#3096=ORIENTED_EDGE('',*,*,#2496,.F.);
#3097=ORIENTED_EDGE('',*,*,#2495,.T.);
#3098=ORIENTED_EDGE('',*,*,#2498,.F.);
#3099=ORIENTED_EDGE('',*,*,#2499,.T.);
#3100=ORIENTED_EDGE('',*,*,#2500,.F.);
#3101=ORIENTED_EDGE('',*,*,#2499,.F.);
#3102=ORIENTED_EDGE('',*,*,#2498,.T.);
#3103=ORIENTED_EDGE('',*,*,#2501,.T.);
#3104=ORIENTED_EDGE('',*,*,#2502,.T.);
#3105=ORIENTED_EDGE('',*,*,#2503,.F.);
#3106=ORIENTED_EDGE('',*,*,#2504,.F.);
#3107=ORIENTED_EDGE('',*,*,#2505,.T.);
#3108=ORIENTED_EDGE('',*,*,#2504,.T.);
#3109=ORIENTED_EDGE('',*,*,#2506,.F.);
#3110=ORIENTED_EDGE('',*,*,#2507,.F.);
#3111=ORIENTED_EDGE('',*,*,#2508,.T.);
#3112=ORIENTED_EDGE('',*,*,#2507,.T.);
#3113=ORIENTED_EDGE('',*,*,#2509,.F.);
#3114=ORIENTED_EDGE('',*,*,#2510,.F.);
#3115=ORIENTED_EDGE('',*,*,#2511,.T.);
#3116=ORIENTED_EDGE('',*,*,#2510,.T.);
#3117=ORIENTED_EDGE('',*,*,#2512,.F.);
#3118=ORIENTED_EDGE('',*,*,#2502,.F.);
#3119=ORIENTED_EDGE('',*,*,#2512,.T.);
#3120=ORIENTED_EDGE('',*,*,#2509,.T.);
#3121=ORIENTED_EDGE('',*,*,#2506,.T.);
#3122=ORIENTED_EDGE('',*,*,#2503,.T.);
#3123=ORIENTED_EDGE('',*,*,#2497,.T.);
#3124=ORIENTED_EDGE('',*,*,#2500,.T.);
#3125=ORIENTED_EDGE('',*,*,#2511,.F.);
#3126=ORIENTED_EDGE('',*,*,#2501,.F.);
#3127=ORIENTED_EDGE('',*,*,#2505,.F.);
#3128=ORIENTED_EDGE('',*,*,#2508,.F.);
#3129=ORIENTED_EDGE('',*,*,#2513,.T.);
#3130=ORIENTED_EDGE('',*,*,#2514,.T.);
#3131=ORIENTED_EDGE('',*,*,#2515,.F.);
#3132=ORIENTED_EDGE('',*,*,#2516,.F.);
#3133=ORIENTED_EDGE('',*,*,#2517,.T.);
#3134=ORIENTED_EDGE('',*,*,#2516,.T.);
#3135=ORIENTED_EDGE('',*,*,#2518,.F.);
#3136=ORIENTED_EDGE('',*,*,#2519,.F.);
#3137=ORIENTED_EDGE('',*,*,#2520,.T.);
#3138=ORIENTED_EDGE('',*,*,#2519,.T.);
#3139=ORIENTED_EDGE('',*,*,#2521,.F.);
#3140=ORIENTED_EDGE('',*,*,#2522,.F.);
#3141=ORIENTED_EDGE('',*,*,#2523,.T.);
#3142=ORIENTED_EDGE('',*,*,#2522,.T.);
#3143=ORIENTED_EDGE('',*,*,#2524,.F.);
#3144=ORIENTED_EDGE('',*,*,#2514,.F.);
#3145=ORIENTED_EDGE('',*,*,#2524,.T.);
#3146=ORIENTED_EDGE('',*,*,#2521,.T.);
#3147=ORIENTED_EDGE('',*,*,#2518,.T.);
#3148=ORIENTED_EDGE('',*,*,#2515,.T.);
#3149=ORIENTED_EDGE('',*,*,#2523,.F.);
#3150=ORIENTED_EDGE('',*,*,#2513,.F.);
#3151=ORIENTED_EDGE('',*,*,#2517,.F.);
#3152=ORIENTED_EDGE('',*,*,#2520,.F.);
#3153=ORIENTED_EDGE('',*,*,#2525,.F.);
#3154=ORIENTED_EDGE('',*,*,#2526,.T.);
#3155=ORIENTED_EDGE('',*,*,#2527,.T.);
#3156=ORIENTED_EDGE('',*,*,#2526,.F.);
#3157=ORIENTED_EDGE('',*,*,#2528,.F.);
#3158=ORIENTED_EDGE('',*,*,#2529,.T.);
#3159=ORIENTED_EDGE('',*,*,#2530,.T.);
#3160=ORIENTED_EDGE('',*,*,#2529,.F.);
#3161=ORIENTED_EDGE('',*,*,#2528,.T.);
#3162=ORIENTED_EDGE('',*,*,#2525,.T.);
#3163=ORIENTED_EDGE('',*,*,#2530,.F.);
#3164=ORIENTED_EDGE('',*,*,#2527,.F.);
#3165=ORIENTED_EDGE('',*,*,#2531,.F.);
#3166=ORIENTED_EDGE('',*,*,#2532,.T.);
#3167=ORIENTED_EDGE('',*,*,#2533,.T.);
#3168=ORIENTED_EDGE('',*,*,#2532,.F.);
#3169=ORIENTED_EDGE('',*,*,#2534,.F.);
#3170=ORIENTED_EDGE('',*,*,#2535,.T.);
#3171=ORIENTED_EDGE('',*,*,#2536,.T.);
#3172=ORIENTED_EDGE('',*,*,#2535,.F.);
#3173=ORIENTED_EDGE('',*,*,#2534,.T.);
#3174=ORIENTED_EDGE('',*,*,#2531,.T.);
#3175=ORIENTED_EDGE('',*,*,#2536,.F.);
#3176=ORIENTED_EDGE('',*,*,#2533,.F.);
#3177=ORIENTED_EDGE('',*,*,#2537,.F.);
#3178=ORIENTED_EDGE('',*,*,#2538,.T.);
#3179=ORIENTED_EDGE('',*,*,#2539,.T.);
#3180=ORIENTED_EDGE('',*,*,#2538,.F.);
#3181=ORIENTED_EDGE('',*,*,#2540,.F.);
#3182=ORIENTED_EDGE('',*,*,#2541,.T.);
#3183=ORIENTED_EDGE('',*,*,#2542,.T.);
#3184=ORIENTED_EDGE('',*,*,#2541,.F.);
#3185=ORIENTED_EDGE('',*,*,#2540,.T.);
#3186=ORIENTED_EDGE('',*,*,#2537,.T.);
#3187=ORIENTED_EDGE('',*,*,#2542,.F.);
#3188=ORIENTED_EDGE('',*,*,#2539,.F.);
#3189=ORIENTED_EDGE('',*,*,#2543,.F.);
#3190=ORIENTED_EDGE('',*,*,#2544,.T.);
#3191=ORIENTED_EDGE('',*,*,#2545,.T.);
#3192=ORIENTED_EDGE('',*,*,#2544,.F.);
#3193=ORIENTED_EDGE('',*,*,#2546,.F.);
#3194=ORIENTED_EDGE('',*,*,#2547,.T.);
#3195=ORIENTED_EDGE('',*,*,#2548,.T.);
#3196=ORIENTED_EDGE('',*,*,#2547,.F.);
#3197=ORIENTED_EDGE('',*,*,#2546,.T.);
#3198=ORIENTED_EDGE('',*,*,#2543,.T.);
#3199=ORIENTED_EDGE('',*,*,#2548,.F.);
#3200=ORIENTED_EDGE('',*,*,#2545,.F.);
#3201=ORIENTED_EDGE('',*,*,#2549,.F.);
#3202=ORIENTED_EDGE('',*,*,#2550,.T.);
#3203=ORIENTED_EDGE('',*,*,#2551,.T.);
#3204=ORIENTED_EDGE('',*,*,#2550,.F.);
#3205=ORIENTED_EDGE('',*,*,#2552,.F.);
#3206=ORIENTED_EDGE('',*,*,#2553,.T.);
#3207=ORIENTED_EDGE('',*,*,#2554,.T.);
#3208=ORIENTED_EDGE('',*,*,#2553,.F.);
#3209=ORIENTED_EDGE('',*,*,#2552,.T.);
#3210=ORIENTED_EDGE('',*,*,#2549,.T.);
#3211=ORIENTED_EDGE('',*,*,#2554,.F.);
#3212=ORIENTED_EDGE('',*,*,#2551,.F.);
#3213=ORIENTED_EDGE('',*,*,#2555,.F.);
#3214=ORIENTED_EDGE('',*,*,#2556,.T.);
#3215=ORIENTED_EDGE('',*,*,#2557,.T.);
#3216=ORIENTED_EDGE('',*,*,#2556,.F.);
#3217=ORIENTED_EDGE('',*,*,#2558,.F.);
#3218=ORIENTED_EDGE('',*,*,#2559,.T.);
#3219=ORIENTED_EDGE('',*,*,#2560,.T.);
#3220=ORIENTED_EDGE('',*,*,#2559,.F.);
#3221=ORIENTED_EDGE('',*,*,#2558,.T.);
#3222=ORIENTED_EDGE('',*,*,#2555,.T.);
#3223=ORIENTED_EDGE('',*,*,#2560,.F.);
#3224=ORIENTED_EDGE('',*,*,#2557,.F.);
#3225=ORIENTED_EDGE('',*,*,#2561,.F.);
#3226=ORIENTED_EDGE('',*,*,#2562,.T.);
#3227=ORIENTED_EDGE('',*,*,#2563,.T.);
#3228=ORIENTED_EDGE('',*,*,#2562,.F.);
#3229=ORIENTED_EDGE('',*,*,#2564,.F.);
#3230=ORIENTED_EDGE('',*,*,#2565,.T.);
#3231=ORIENTED_EDGE('',*,*,#2566,.T.);
#3232=ORIENTED_EDGE('',*,*,#2565,.F.);
#3233=ORIENTED_EDGE('',*,*,#2564,.T.);
#3234=ORIENTED_EDGE('',*,*,#2561,.T.);
#3235=ORIENTED_EDGE('',*,*,#2566,.F.);
#3236=ORIENTED_EDGE('',*,*,#2563,.F.);
#3237=ORIENTED_EDGE('',*,*,#2567,.F.);
#3238=ORIENTED_EDGE('',*,*,#2568,.F.);
#3239=ORIENTED_EDGE('',*,*,#2569,.T.);
#3240=ORIENTED_EDGE('',*,*,#2567,.T.);
#3241=ORIENTED_EDGE('',*,*,#2569,.F.);
#3242=ORIENTED_EDGE('',*,*,#2570,.F.);
#3243=ORIENTED_EDGE('',*,*,#2571,.T.);
#3244=ORIENTED_EDGE('',*,*,#2568,.T.);
#3245=ORIENTED_EDGE('',*,*,#2571,.F.);
#3246=ORIENTED_EDGE('',*,*,#2572,.F.);
#3247=ORIENTED_EDGE('',*,*,#2573,.T.);
#3248=ORIENTED_EDGE('',*,*,#2570,.T.);
#3249=ORIENTED_EDGE('',*,*,#2573,.F.);
#3250=ORIENTED_EDGE('',*,*,#2572,.T.);
#3251=ORIENTED_EDGE('',*,*,#2574,.F.);
#3252=ORIENTED_EDGE('',*,*,#2575,.F.);
#3253=ORIENTED_EDGE('',*,*,#2576,.T.);
#3254=ORIENTED_EDGE('',*,*,#2574,.T.);
#3255=ORIENTED_EDGE('',*,*,#2576,.F.);
#3256=ORIENTED_EDGE('',*,*,#2577,.F.);
#3257=ORIENTED_EDGE('',*,*,#2578,.T.);
#3258=ORIENTED_EDGE('',*,*,#2575,.T.);
#3259=ORIENTED_EDGE('',*,*,#2578,.F.);
#3260=ORIENTED_EDGE('',*,*,#2579,.F.);
#3261=ORIENTED_EDGE('',*,*,#2580,.T.);
#3262=ORIENTED_EDGE('',*,*,#2577,.T.);
#3263=ORIENTED_EDGE('',*,*,#2580,.F.);
#3264=ORIENTED_EDGE('',*,*,#2579,.T.);
#3265=ORIENTED_EDGE('',*,*,#2581,.T.);
#3266=ORIENTED_EDGE('',*,*,#2582,.T.);
#3267=ORIENTED_EDGE('',*,*,#2583,.T.);
#3268=ORIENTED_EDGE('',*,*,#2584,.F.);
#3269=ORIENTED_EDGE('',*,*,#2585,.T.);
#3270=ORIENTED_EDGE('',*,*,#2586,.T.);
#3271=ORIENTED_EDGE('',*,*,#2587,.T.);
#3272=ORIENTED_EDGE('',*,*,#2582,.F.);
#3273=ORIENTED_EDGE('',*,*,#2588,.T.);
#3274=ORIENTED_EDGE('',*,*,#2589,.T.);
#3275=ORIENTED_EDGE('',*,*,#2590,.T.);
#3276=ORIENTED_EDGE('',*,*,#2586,.F.);
#3277=ORIENTED_EDGE('',*,*,#2591,.T.);
#3278=ORIENTED_EDGE('',*,*,#2592,.T.);
#3279=ORIENTED_EDGE('',*,*,#2593,.T.);
#3280=ORIENTED_EDGE('',*,*,#2589,.F.);
#3281=ORIENTED_EDGE('',*,*,#2594,.T.);
#3282=ORIENTED_EDGE('',*,*,#2595,.T.);
#3283=ORIENTED_EDGE('',*,*,#2596,.T.);
#3284=ORIENTED_EDGE('',*,*,#2592,.F.);
#3285=ORIENTED_EDGE('',*,*,#2597,.T.);
#3286=ORIENTED_EDGE('',*,*,#2584,.T.);
#3287=ORIENTED_EDGE('',*,*,#2598,.T.);
#3288=ORIENTED_EDGE('',*,*,#2595,.F.);
#3289=ORIENTED_EDGE('',*,*,#2597,.F.);
#3290=ORIENTED_EDGE('',*,*,#2594,.F.);
#3291=ORIENTED_EDGE('',*,*,#2591,.F.);
#3292=ORIENTED_EDGE('',*,*,#2588,.F.);
#3293=ORIENTED_EDGE('',*,*,#2585,.F.);
#3294=ORIENTED_EDGE('',*,*,#2581,.F.);
#3295=ORIENTED_EDGE('',*,*,#2598,.F.);
#3296=ORIENTED_EDGE('',*,*,#2583,.F.);
#3297=ORIENTED_EDGE('',*,*,#2587,.F.);
#3298=ORIENTED_EDGE('',*,*,#2590,.F.);
#3299=ORIENTED_EDGE('',*,*,#2593,.F.);
#3300=ORIENTED_EDGE('',*,*,#2596,.F.);
#3301=ORIENTED_EDGE('',*,*,#2599,.F.);
#3302=ORIENTED_EDGE('',*,*,#2600,.T.);
#3303=ORIENTED_EDGE('',*,*,#2601,.F.);
#3304=ORIENTED_EDGE('',*,*,#2600,.F.);
#3305=ORIENTED_EDGE('',*,*,#2602,.F.);
#3306=ORIENTED_EDGE('',*,*,#2603,.T.);
#3307=ORIENTED_EDGE('',*,*,#2604,.F.);
#3308=ORIENTED_EDGE('',*,*,#2603,.F.);
#3309=ORIENTED_EDGE('',*,*,#2605,.T.);
#3310=ORIENTED_EDGE('',*,*,#2605,.F.);
#3311=ORIENTED_EDGE('',*,*,#2602,.T.);
#3312=ORIENTED_EDGE('',*,*,#2601,.T.);
#3313=ORIENTED_EDGE('',*,*,#2606,.F.);
#3314=ORIENTED_EDGE('',*,*,#2607,.T.);
#3315=ORIENTED_EDGE('',*,*,#2608,.F.);
#3316=ORIENTED_EDGE('',*,*,#2609,.F.);
#3317=ORIENTED_EDGE('',*,*,#2610,.F.);
#3318=ORIENTED_EDGE('',*,*,#2611,.T.);
#3319=ORIENTED_EDGE('',*,*,#2612,.F.);
#3320=ORIENTED_EDGE('',*,*,#2613,.F.);
#3321=ORIENTED_EDGE('',*,*,#2614,.T.);
#3322=ORIENTED_EDGE('',*,*,#2615,.F.);
#3323=ORIENTED_EDGE('',*,*,#2614,.F.);
#3324=ORIENTED_EDGE('',*,*,#2616,.F.);
#3325=ORIENTED_EDGE('',*,*,#2607,.F.);
#3326=ORIENTED_EDGE('',*,*,#2617,.F.);
#3327=ORIENTED_EDGE('',*,*,#2618,.T.);
#3328=ORIENTED_EDGE('',*,*,#2619,.F.);
#3329=ORIENTED_EDGE('',*,*,#2620,.F.);
#3330=ORIENTED_EDGE('',*,*,#2611,.F.);
#3331=ORIENTED_EDGE('',*,*,#2621,.F.);
#3332=ORIENTED_EDGE('',*,*,#2618,.F.);
#3333=ORIENTED_EDGE('',*,*,#2622,.T.);
#3334=ORIENTED_EDGE('',*,*,#2623,.T.);
#3335=ORIENTED_EDGE('',*,*,#2624,.T.);
#3336=ORIENTED_EDGE('',*,*,#2625,.T.);
#3337=ORIENTED_EDGE('',*,*,#2626,.T.);
#3338=ORIENTED_EDGE('',*,*,#2627,.T.);
#3339=ORIENTED_EDGE('',*,*,#2609,.T.);
#3340=ORIENTED_EDGE('',*,*,#2620,.T.);
#3341=ORIENTED_EDGE('',*,*,#2617,.T.);
#3342=ORIENTED_EDGE('',*,*,#2628,.T.);
#3343=ORIENTED_EDGE('',*,*,#2629,.T.);
#3344=ORIENTED_EDGE('',*,*,#2630,.T.);
#3345=ORIENTED_EDGE('',*,*,#2612,.T.);
#3346=ORIENTED_EDGE('',*,*,#2615,.T.);
#3347=ORIENTED_EDGE('',*,*,#2606,.T.);
#3348=ORIENTED_EDGE('',*,*,#2631,.T.);
#3349=ORIENTED_EDGE('',*,*,#2632,.T.);
#3350=ORIENTED_EDGE('',*,*,#2633,.T.);
#3351=ORIENTED_EDGE('',*,*,#2610,.T.);
#3352=ORIENTED_EDGE('',*,*,#2633,.F.);
#3353=ORIENTED_EDGE('',*,*,#2634,.F.);
#3354=ORIENTED_EDGE('',*,*,#2631,.F.);
#3355=ORIENTED_EDGE('',*,*,#2608,.T.);
#3356=ORIENTED_EDGE('',*,*,#2616,.T.);
#3357=ORIENTED_EDGE('',*,*,#2613,.T.);
#3358=ORIENTED_EDGE('',*,*,#2630,.F.);
#3359=ORIENTED_EDGE('',*,*,#2635,.F.);
#3360=ORIENTED_EDGE('',*,*,#2628,.F.);
#3361=ORIENTED_EDGE('',*,*,#2619,.T.);
#3362=ORIENTED_EDGE('',*,*,#2621,.T.);
#3363=ORIENTED_EDGE('',*,*,#2629,.F.);
#3364=ORIENTED_EDGE('',*,*,#2635,.T.);
#3365=ORIENTED_EDGE('',*,*,#2599,.T.);
#3366=ORIENTED_EDGE('',*,*,#2632,.F.);
#3367=ORIENTED_EDGE('',*,*,#2634,.T.);
#3368=ORIENTED_EDGE('',*,*,#2604,.T.);
#3369=ORIENTED_EDGE('',*,*,#2636,.F.);
#3370=ORIENTED_EDGE('',*,*,#2637,.T.);
#3371=ORIENTED_EDGE('',*,*,#2638,.T.);
#3372=ORIENTED_EDGE('',*,*,#2639,.F.);
#3373=ORIENTED_EDGE('',*,*,#2640,.F.);
#3374=ORIENTED_EDGE('',*,*,#2641,.T.);
#3375=ORIENTED_EDGE('',*,*,#2642,.T.);
#3376=ORIENTED_EDGE('',*,*,#2637,.F.);
#3377=ORIENTED_EDGE('',*,*,#2643,.F.);
#3378=ORIENTED_EDGE('',*,*,#2644,.T.);
#3379=ORIENTED_EDGE('',*,*,#2645,.T.);
#3380=ORIENTED_EDGE('',*,*,#2641,.F.);
#3381=ORIENTED_EDGE('',*,*,#2646,.F.);
#3382=ORIENTED_EDGE('',*,*,#2639,.T.);
#3383=ORIENTED_EDGE('',*,*,#2647,.T.);
#3384=ORIENTED_EDGE('',*,*,#2644,.F.);
#3385=ORIENTED_EDGE('',*,*,#2647,.F.);
#3386=ORIENTED_EDGE('',*,*,#2638,.F.);
#3387=ORIENTED_EDGE('',*,*,#2642,.F.);
#3388=ORIENTED_EDGE('',*,*,#2645,.F.);
#3389=ORIENTED_EDGE('',*,*,#2648,.F.);
#3390=ORIENTED_EDGE('',*,*,#2649,.T.);
#3391=ORIENTED_EDGE('',*,*,#2627,.F.);
#3392=ORIENTED_EDGE('',*,*,#2649,.F.);
#3393=ORIENTED_EDGE('',*,*,#2650,.F.);
#3394=ORIENTED_EDGE('',*,*,#2651,.T.);
#3395=ORIENTED_EDGE('',*,*,#2626,.F.);
#3396=ORIENTED_EDGE('',*,*,#2651,.F.);
#3397=ORIENTED_EDGE('',*,*,#2652,.T.);
#3398=ORIENTED_EDGE('',*,*,#2653,.T.);
#3399=ORIENTED_EDGE('',*,*,#2625,.F.);
#3400=ORIENTED_EDGE('',*,*,#2654,.F.);
#3401=ORIENTED_EDGE('',*,*,#2655,.T.);
#3402=ORIENTED_EDGE('',*,*,#2654,.T.);
#3403=ORIENTED_EDGE('',*,*,#2624,.F.);
#3404=ORIENTED_EDGE('',*,*,#2656,.F.);
#3405=ORIENTED_EDGE('',*,*,#2657,.T.);
#3406=ORIENTED_EDGE('',*,*,#2656,.T.);
#3407=ORIENTED_EDGE('',*,*,#2623,.F.);
#3408=ORIENTED_EDGE('',*,*,#2658,.F.);
#3409=ORIENTED_EDGE('',*,*,#2659,.T.);
#3410=ORIENTED_EDGE('',*,*,#2658,.T.);
#3411=ORIENTED_EDGE('',*,*,#2622,.F.);
#3412=ORIENTED_EDGE('',*,*,#2653,.F.);
#3413=ORIENTED_EDGE('',*,*,#2659,.F.);
#3414=ORIENTED_EDGE('',*,*,#2652,.F.);
#3415=ORIENTED_EDGE('',*,*,#2655,.F.);
#3416=ORIENTED_EDGE('',*,*,#2657,.F.);
#3417=ORIENTED_EDGE('',*,*,#2636,.T.);
#3418=ORIENTED_EDGE('',*,*,#2646,.T.);
#3419=ORIENTED_EDGE('',*,*,#2643,.T.);
#3420=ORIENTED_EDGE('',*,*,#2640,.T.);
#3421=ORIENTED_EDGE('',*,*,#2648,.T.);
#3422=ORIENTED_EDGE('',*,*,#2650,.T.);
#3423=ORIENTED_EDGE('',*,*,#2660,.T.);
#3424=ORIENTED_EDGE('',*,*,#2661,.T.);
#3425=ORIENTED_EDGE('',*,*,#2662,.F.);
#3426=ORIENTED_EDGE('',*,*,#2661,.F.);
#3427=ORIENTED_EDGE('',*,*,#2663,.F.);
#3428=ORIENTED_EDGE('',*,*,#2662,.T.);
#3429=ORIENTED_EDGE('',*,*,#2664,.T.);
#3430=ORIENTED_EDGE('',*,*,#2664,.F.);
#3431=ORIENTED_EDGE('',*,*,#2663,.T.);
#3432=ORIENTED_EDGE('',*,*,#2665,.F.);
#3433=ORIENTED_EDGE('',*,*,#2665,.T.);
#3434=ORIENTED_EDGE('',*,*,#2660,.F.);
#3435=ORIENTED_EDGE('',*,*,#2666,.F.);
#3436=ORIENTED_EDGE('',*,*,#2667,.F.);
#3437=ORIENTED_EDGE('',*,*,#2668,.F.);
#3438=ORIENTED_EDGE('',*,*,#2669,.T.);
#3439=ORIENTED_EDGE('',*,*,#2670,.F.);
#3440=ORIENTED_EDGE('',*,*,#2669,.F.);
#3441=ORIENTED_EDGE('',*,*,#2671,.F.);
#3442=ORIENTED_EDGE('',*,*,#2672,.T.);
#3443=ORIENTED_EDGE('',*,*,#2673,.F.);
#3444=ORIENTED_EDGE('',*,*,#2674,.F.);
#3445=ORIENTED_EDGE('',*,*,#2675,.F.);
#3446=ORIENTED_EDGE('',*,*,#2672,.F.);
#3447=ORIENTED_EDGE('',*,*,#2676,.F.);
#3448=ORIENTED_EDGE('',*,*,#2677,.T.);
#3449=ORIENTED_EDGE('',*,*,#2678,.T.);
#3450=ORIENTED_EDGE('',*,*,#2677,.F.);
#3451=ORIENTED_EDGE('',*,*,#2667,.T.);
#3452=ORIENTED_EDGE('',*,*,#2666,.T.);
#3453=ORIENTED_EDGE('',*,*,#2668,.T.);
#3454=ORIENTED_EDGE('',*,*,#2674,.T.);
#3455=ORIENTED_EDGE('',*,*,#2673,.T.);
#3456=ORIENTED_EDGE('',*,*,#2675,.T.);
#3457=ORIENTED_EDGE('',*,*,#2679,.T.);
#3458=ORIENTED_EDGE('',*,*,#2680,.T.);
#3459=ORIENTED_EDGE('',*,*,#2681,.T.);
#3460=ORIENTED_EDGE('',*,*,#2682,.T.);
#3461=ORIENTED_EDGE('',*,*,#2683,.T.);
#3462=ORIENTED_EDGE('',*,*,#2684,.T.);
#3463=ORIENTED_EDGE('',*,*,#2685,.T.);
#3464=ORIENTED_EDGE('',*,*,#2686,.T.);
#3465=ORIENTED_EDGE('',*,*,#2687,.T.);
#3466=ORIENTED_EDGE('',*,*,#2688,.T.);
#3467=ORIENTED_EDGE('',*,*,#2689,.T.);
#3468=ORIENTED_EDGE('',*,*,#2690,.T.);
#3469=ORIENTED_EDGE('',*,*,#2680,.F.);
#3470=ORIENTED_EDGE('',*,*,#2679,.F.);
#3471=ORIENTED_EDGE('',*,*,#2681,.F.);
#3472=ORIENTED_EDGE('',*,*,#2691,.T.);
#3473=ORIENTED_EDGE('',*,*,#2692,.F.);
#3474=ORIENTED_EDGE('',*,*,#2691,.F.);
#3475=ORIENTED_EDGE('',*,*,#2693,.F.);
#3476=ORIENTED_EDGE('',*,*,#2694,.T.);
#3477=ORIENTED_EDGE('',*,*,#2683,.F.);
#3478=ORIENTED_EDGE('',*,*,#2682,.F.);
#3479=ORIENTED_EDGE('',*,*,#2684,.F.);
#3480=ORIENTED_EDGE('',*,*,#2694,.F.);
#3481=ORIENTED_EDGE('',*,*,#2686,.F.);
#3482=ORIENTED_EDGE('',*,*,#2685,.F.);
#3483=ORIENTED_EDGE('',*,*,#2687,.F.);
#3484=ORIENTED_EDGE('',*,*,#2695,.T.);
#3485=ORIENTED_EDGE('',*,*,#2696,.F.);
#3486=ORIENTED_EDGE('',*,*,#2695,.F.);
#3487=ORIENTED_EDGE('',*,*,#2697,.F.);
#3488=ORIENTED_EDGE('',*,*,#2698,.T.);
#3489=ORIENTED_EDGE('',*,*,#2689,.F.);
#3490=ORIENTED_EDGE('',*,*,#2688,.F.);
#3491=ORIENTED_EDGE('',*,*,#2690,.F.);
#3492=ORIENTED_EDGE('',*,*,#2698,.F.);
#3493=ORIENTED_EDGE('',*,*,#2678,.F.);
#3494=ORIENTED_EDGE('',*,*,#2699,.T.);
#3495=ORIENTED_EDGE('',*,*,#2700,.F.);
#3496=ORIENTED_EDGE('',*,*,#2676,.T.);
#3497=ORIENTED_EDGE('',*,*,#2701,.F.);
#3498=ORIENTED_EDGE('',*,*,#2702,.T.);
#3499=ORIENTED_EDGE('',*,*,#2700,.T.);
#3500=ORIENTED_EDGE('',*,*,#2702,.F.);
#3501=ORIENTED_EDGE('',*,*,#2701,.T.);
#3502=ORIENTED_EDGE('',*,*,#2703,.F.);
#3503=ORIENTED_EDGE('',*,*,#2703,.T.);
#3504=ORIENTED_EDGE('',*,*,#2704,.T.);
#3505=ORIENTED_EDGE('',*,*,#2699,.F.);
#3506=ORIENTED_EDGE('',*,*,#2704,.F.);
#3507=ORIENTED_EDGE('',*,*,#2671,.T.);
#3508=ORIENTED_EDGE('',*,*,#2670,.T.);
#3509=ORIENTED_EDGE('',*,*,#2693,.T.);
#3510=ORIENTED_EDGE('',*,*,#2692,.T.);
#3511=ORIENTED_EDGE('',*,*,#2697,.T.);
#3512=ORIENTED_EDGE('',*,*,#2696,.T.);
#3513=ORIENTED_EDGE('',*,*,#2705,.F.);
#3514=ORIENTED_EDGE('',*,*,#2706,.T.);
#3515=ORIENTED_EDGE('',*,*,#2707,.T.);
#3516=ORIENTED_EDGE('',*,*,#2706,.F.);
#3517=ORIENTED_EDGE('',*,*,#2708,.F.);
#3518=ORIENTED_EDGE('',*,*,#2709,.T.);
#3519=ORIENTED_EDGE('',*,*,#2710,.T.);
#3520=ORIENTED_EDGE('',*,*,#2709,.F.);
#3521=ORIENTED_EDGE('',*,*,#2708,.T.);
#3522=ORIENTED_EDGE('',*,*,#2705,.T.);
#3523=ORIENTED_EDGE('',*,*,#2710,.F.);
#3524=ORIENTED_EDGE('',*,*,#2707,.F.);
#3525=ORIENTED_EDGE('',*,*,#2711,.T.);
#3526=ORIENTED_EDGE('',*,*,#2712,.T.);
#3527=ORIENTED_EDGE('',*,*,#2713,.T.);
#3528=ORIENTED_EDGE('',*,*,#2714,.F.);
#3529=ORIENTED_EDGE('',*,*,#2715,.T.);
#3530=ORIENTED_EDGE('',*,*,#2716,.T.);
#3531=ORIENTED_EDGE('',*,*,#2717,.T.);
#3532=ORIENTED_EDGE('',*,*,#2712,.F.);
#3533=ORIENTED_EDGE('',*,*,#2718,.T.);
#3534=ORIENTED_EDGE('',*,*,#2719,.T.);
#3535=ORIENTED_EDGE('',*,*,#2720,.T.);
#3536=ORIENTED_EDGE('',*,*,#2716,.F.);
#3537=ORIENTED_EDGE('',*,*,#2721,.T.);
#3538=ORIENTED_EDGE('',*,*,#2722,.T.);
#3539=ORIENTED_EDGE('',*,*,#2723,.T.);
#3540=ORIENTED_EDGE('',*,*,#2719,.F.);
#3541=ORIENTED_EDGE('',*,*,#2724,.T.);
#3542=ORIENTED_EDGE('',*,*,#2725,.T.);
#3543=ORIENTED_EDGE('',*,*,#2726,.T.);
#3544=ORIENTED_EDGE('',*,*,#2722,.F.);
#3545=ORIENTED_EDGE('',*,*,#2727,.T.);
#3546=ORIENTED_EDGE('',*,*,#2714,.T.);
#3547=ORIENTED_EDGE('',*,*,#2728,.T.);
#3548=ORIENTED_EDGE('',*,*,#2725,.F.);
#3549=ORIENTED_EDGE('',*,*,#2727,.F.);
#3550=ORIENTED_EDGE('',*,*,#2724,.F.);
#3551=ORIENTED_EDGE('',*,*,#2721,.F.);
#3552=ORIENTED_EDGE('',*,*,#2718,.F.);
#3553=ORIENTED_EDGE('',*,*,#2715,.F.);
#3554=ORIENTED_EDGE('',*,*,#2711,.F.);
#3555=ORIENTED_EDGE('',*,*,#2728,.F.);
#3556=ORIENTED_EDGE('',*,*,#2713,.F.);
#3557=ORIENTED_EDGE('',*,*,#2717,.F.);
#3558=ORIENTED_EDGE('',*,*,#2720,.F.);
#3559=ORIENTED_EDGE('',*,*,#2723,.F.);
#3560=ORIENTED_EDGE('',*,*,#2726,.F.);
#3561=ORIENTED_EDGE('',*,*,#2729,.F.);
#3562=ORIENTED_EDGE('',*,*,#2730,.F.);
#3563=ORIENTED_EDGE('',*,*,#2731,.F.);
#3564=ORIENTED_EDGE('',*,*,#2732,.T.);
#3565=ORIENTED_EDGE('',*,*,#2730,.T.);
#3566=ORIENTED_EDGE('',*,*,#2732,.F.);
#3567=ORIENTED_EDGE('',*,*,#2733,.F.);
#3568=ORIENTED_EDGE('',*,*,#2734,.T.);
#3569=ORIENTED_EDGE('',*,*,#2731,.T.);
#3570=ORIENTED_EDGE('',*,*,#2734,.F.);
#3571=ORIENTED_EDGE('',*,*,#2735,.F.);
#3572=ORIENTED_EDGE('',*,*,#2736,.T.);
#3573=ORIENTED_EDGE('',*,*,#2733,.T.);
#3574=ORIENTED_EDGE('',*,*,#2736,.F.);
#3575=ORIENTED_EDGE('',*,*,#2735,.T.);
#3576=ORIENTED_EDGE('',*,*,#2737,.F.);
#3577=ORIENTED_EDGE('',*,*,#2738,.F.);
#3578=ORIENTED_EDGE('',*,*,#2739,.T.);
#3579=ORIENTED_EDGE('',*,*,#2737,.T.);
#3580=ORIENTED_EDGE('',*,*,#2739,.F.);
#3581=ORIENTED_EDGE('',*,*,#2729,.T.);
#3582=ORIENTED_EDGE('',*,*,#2740,.T.);
#3583=ORIENTED_EDGE('',*,*,#2738,.T.);
#3584=ORIENTED_EDGE('',*,*,#2740,.F.);
#3585=ORIENTED_EDGE('',*,*,#2741,.F.);
#3586=ORIENTED_EDGE('',*,*,#2742,.T.);
#3587=ORIENTED_EDGE('',*,*,#2743,.F.);
#3588=ORIENTED_EDGE('',*,*,#2742,.F.);
#3589=ORIENTED_EDGE('',*,*,#2741,.T.);
#3590=ORIENTED_EDGE('',*,*,#2744,.F.);
#3591=ORIENTED_EDGE('',*,*,#2745,.T.);
#3592=ORIENTED_EDGE('',*,*,#2746,.T.);
#3593=ORIENTED_EDGE('',*,*,#2745,.F.);
#3594=ORIENTED_EDGE('',*,*,#2746,.F.);
#3595=ORIENTED_EDGE('',*,*,#2747,.F.);
#3596=ORIENTED_EDGE('',*,*,#2748,.T.);
#3597=ORIENTED_EDGE('',*,*,#2749,.F.);
#3598=ORIENTED_EDGE('',*,*,#2750,.T.);
#3599=ORIENTED_EDGE('',*,*,#2751,.F.);
#3600=ORIENTED_EDGE('',*,*,#2750,.F.);
#3601=ORIENTED_EDGE('',*,*,#2752,.F.);
#3602=ORIENTED_EDGE('',*,*,#2753,.F.);
#3603=ORIENTED_EDGE('',*,*,#2754,.F.);
#3604=ORIENTED_EDGE('',*,*,#2753,.T.);
#3605=ORIENTED_EDGE('',*,*,#2755,.T.);
#3606=ORIENTED_EDGE('',*,*,#2756,.T.);
#3607=ORIENTED_EDGE('',*,*,#2752,.T.);
#3608=ORIENTED_EDGE('',*,*,#2749,.T.);
#3609=ORIENTED_EDGE('',*,*,#2757,.T.);
#3610=ORIENTED_EDGE('',*,*,#2755,.F.);
#3611=ORIENTED_EDGE('',*,*,#2758,.F.);
#3612=ORIENTED_EDGE('',*,*,#2756,.F.);
#3613=ORIENTED_EDGE('',*,*,#2757,.F.);
#3614=ORIENTED_EDGE('',*,*,#2748,.F.);
#3615=ORIENTED_EDGE('',*,*,#2759,.F.);
#3616=ORIENTED_EDGE('',*,*,#2760,.T.);
#3617=ORIENTED_EDGE('',*,*,#2761,.F.);
#3618=ORIENTED_EDGE('',*,*,#2762,.T.);
#3619=ORIENTED_EDGE('',*,*,#2763,.F.);
#3620=ORIENTED_EDGE('',*,*,#2762,.F.);
#3621=ORIENTED_EDGE('',*,*,#2764,.F.);
#3622=ORIENTED_EDGE('',*,*,#2765,.F.);
#3623=ORIENTED_EDGE('',*,*,#2766,.F.);
#3624=ORIENTED_EDGE('',*,*,#2765,.T.);
#3625=ORIENTED_EDGE('',*,*,#2767,.T.);
#3626=ORIENTED_EDGE('',*,*,#2768,.T.);
#3627=ORIENTED_EDGE('',*,*,#2764,.T.);
#3628=ORIENTED_EDGE('',*,*,#2761,.T.);
#3629=ORIENTED_EDGE('',*,*,#2769,.T.);
#3630=ORIENTED_EDGE('',*,*,#2767,.F.);
#3631=ORIENTED_EDGE('',*,*,#2770,.F.);
#3632=ORIENTED_EDGE('',*,*,#2768,.F.);
#3633=ORIENTED_EDGE('',*,*,#2769,.F.);
#3634=ORIENTED_EDGE('',*,*,#2760,.F.);
#3635=ORIENTED_EDGE('',*,*,#2771,.F.);
#3636=ORIENTED_EDGE('',*,*,#2772,.T.);
#3637=ORIENTED_EDGE('',*,*,#2773,.T.);
#3638=ORIENTED_EDGE('',*,*,#2772,.F.);
#3639=ORIENTED_EDGE('',*,*,#2754,.T.);
#3640=ORIENTED_EDGE('',*,*,#2758,.T.);
#3641=ORIENTED_EDGE('',*,*,#2747,.T.);
#3642=ORIENTED_EDGE('',*,*,#2751,.T.);
#3643=ORIENTED_EDGE('',*,*,#2766,.T.);
#3644=ORIENTED_EDGE('',*,*,#2770,.T.);
#3645=ORIENTED_EDGE('',*,*,#2759,.T.);
#3646=ORIENTED_EDGE('',*,*,#2763,.T.);
#3647=ORIENTED_EDGE('',*,*,#2771,.T.);
#3648=ORIENTED_EDGE('',*,*,#2743,.T.);
#3649=ORIENTED_EDGE('',*,*,#2773,.F.);
#3650=ORIENTED_EDGE('',*,*,#2744,.T.);
#3651=ORIENTED_EDGE('',*,*,#2774,.F.);
#3652=ORIENTED_EDGE('',*,*,#2775,.T.);
#3653=ORIENTED_EDGE('',*,*,#2776,.F.);
#3654=ORIENTED_EDGE('',*,*,#2777,.F.);
#3655=ORIENTED_EDGE('',*,*,#2778,.T.);
#3656=ORIENTED_EDGE('',*,*,#2779,.F.);
#3657=ORIENTED_EDGE('',*,*,#2780,.F.);
#3658=ORIENTED_EDGE('',*,*,#2778,.F.);
#3659=ORIENTED_EDGE('',*,*,#2781,.F.);
#3660=ORIENTED_EDGE('',*,*,#2782,.F.);
#3661=ORIENTED_EDGE('',*,*,#2775,.F.);
#3662=ORIENTED_EDGE('',*,*,#2783,.F.);
#3663=ORIENTED_EDGE('',*,*,#2781,.T.);
#3664=ORIENTED_EDGE('',*,*,#2777,.T.);
#3665=ORIENTED_EDGE('',*,*,#2784,.F.);
#3666=ORIENTED_EDGE('',*,*,#2785,.T.);
#3667=ORIENTED_EDGE('',*,*,#2786,.F.);
#3668=ORIENTED_EDGE('',*,*,#2787,.F.);
#3669=ORIENTED_EDGE('',*,*,#2788,.F.);
#3670=ORIENTED_EDGE('',*,*,#2789,.T.);
#3671=ORIENTED_EDGE('',*,*,#2790,.F.);
#3672=ORIENTED_EDGE('',*,*,#2785,.F.);
#3673=ORIENTED_EDGE('',*,*,#2791,.F.);
#3674=ORIENTED_EDGE('',*,*,#2792,.F.);
#3675=ORIENTED_EDGE('',*,*,#2793,.F.);
#3676=ORIENTED_EDGE('',*,*,#2789,.F.);
#3677=ORIENTED_EDGE('',*,*,#2794,.T.);
#3678=ORIENTED_EDGE('',*,*,#2786,.T.);
#3679=ORIENTED_EDGE('',*,*,#2790,.T.);
#3680=ORIENTED_EDGE('',*,*,#2793,.T.);
#3681=ORIENTED_EDGE('',*,*,#2795,.T.);
#3682=ORIENTED_EDGE('',*,*,#2787,.T.);
#3683=ORIENTED_EDGE('',*,*,#2795,.F.);
#3684=ORIENTED_EDGE('',*,*,#2792,.T.);
#3685=ORIENTED_EDGE('',*,*,#2796,.T.);
#3686=ORIENTED_EDGE('',*,*,#2782,.T.);
#3687=ORIENTED_EDGE('',*,*,#2783,.T.);
#3688=ORIENTED_EDGE('',*,*,#2776,.T.);
#3689=ORIENTED_EDGE('',*,*,#2774,.T.);
#3690=ORIENTED_EDGE('',*,*,#2794,.F.);
#3691=ORIENTED_EDGE('',*,*,#2797,.T.);
#3692=ORIENTED_EDGE('',*,*,#2798,.T.);
#3693=ORIENTED_EDGE('',*,*,#2797,.F.);
#3694=ORIENTED_EDGE('',*,*,#2779,.T.);
#3695=ORIENTED_EDGE('',*,*,#2780,.T.);
#3696=ORIENTED_EDGE('',*,*,#2798,.F.);
#3697=ORIENTED_EDGE('',*,*,#2784,.T.);
#3698=ORIENTED_EDGE('',*,*,#2796,.F.);
#3699=ORIENTED_EDGE('',*,*,#2791,.T.);
#3700=ORIENTED_EDGE('',*,*,#2788,.T.);
#3701=ORIENTED_EDGE('',*,*,#2799,.F.);
#3702=ORIENTED_EDGE('',*,*,#2800,.T.);
#3703=ORIENTED_EDGE('',*,*,#2801,.F.);
#3704=ORIENTED_EDGE('',*,*,#2802,.F.);
#3705=ORIENTED_EDGE('',*,*,#2803,.T.);
#3706=ORIENTED_EDGE('',*,*,#2804,.F.);
#3707=ORIENTED_EDGE('',*,*,#2805,.F.);
#3708=ORIENTED_EDGE('',*,*,#2803,.F.);
#3709=ORIENTED_EDGE('',*,*,#2806,.F.);
#3710=ORIENTED_EDGE('',*,*,#2807,.F.);
#3711=ORIENTED_EDGE('',*,*,#2800,.F.);
#3712=ORIENTED_EDGE('',*,*,#2808,.F.);
#3713=ORIENTED_EDGE('',*,*,#2806,.T.);
#3714=ORIENTED_EDGE('',*,*,#2802,.T.);
#3715=ORIENTED_EDGE('',*,*,#2809,.F.);
#3716=ORIENTED_EDGE('',*,*,#2810,.T.);
#3717=ORIENTED_EDGE('',*,*,#2811,.F.);
#3718=ORIENTED_EDGE('',*,*,#2812,.F.);
#3719=ORIENTED_EDGE('',*,*,#2813,.F.);
#3720=ORIENTED_EDGE('',*,*,#2814,.T.);
#3721=ORIENTED_EDGE('',*,*,#2815,.F.);
#3722=ORIENTED_EDGE('',*,*,#2810,.F.);
#3723=ORIENTED_EDGE('',*,*,#2816,.F.);
#3724=ORIENTED_EDGE('',*,*,#2817,.F.);
#3725=ORIENTED_EDGE('',*,*,#2818,.F.);
#3726=ORIENTED_EDGE('',*,*,#2814,.F.);
#3727=ORIENTED_EDGE('',*,*,#2819,.T.);
#3728=ORIENTED_EDGE('',*,*,#2811,.T.);
#3729=ORIENTED_EDGE('',*,*,#2815,.T.);
#3730=ORIENTED_EDGE('',*,*,#2818,.T.);
#3731=ORIENTED_EDGE('',*,*,#2820,.T.);
#3732=ORIENTED_EDGE('',*,*,#2812,.T.);
#3733=ORIENTED_EDGE('',*,*,#2820,.F.);
#3734=ORIENTED_EDGE('',*,*,#2817,.T.);
#3735=ORIENTED_EDGE('',*,*,#2821,.T.);
#3736=ORIENTED_EDGE('',*,*,#2807,.T.);
#3737=ORIENTED_EDGE('',*,*,#2808,.T.);
#3738=ORIENTED_EDGE('',*,*,#2801,.T.);
#3739=ORIENTED_EDGE('',*,*,#2799,.T.);
#3740=ORIENTED_EDGE('',*,*,#2819,.F.);
#3741=ORIENTED_EDGE('',*,*,#2822,.T.);
#3742=ORIENTED_EDGE('',*,*,#2823,.T.);
#3743=ORIENTED_EDGE('',*,*,#2822,.F.);
#3744=ORIENTED_EDGE('',*,*,#2804,.T.);
#3745=ORIENTED_EDGE('',*,*,#2805,.T.);
#3746=ORIENTED_EDGE('',*,*,#2823,.F.);
#3747=ORIENTED_EDGE('',*,*,#2809,.T.);
#3748=ORIENTED_EDGE('',*,*,#2821,.F.);
#3749=ORIENTED_EDGE('',*,*,#2816,.T.);
#3750=ORIENTED_EDGE('',*,*,#2813,.T.);
#3751=ORIENTED_EDGE('',*,*,#2824,.F.);
#3752=ORIENTED_EDGE('',*,*,#2825,.T.);
#3753=ORIENTED_EDGE('',*,*,#2826,.F.);
#3754=ORIENTED_EDGE('',*,*,#2827,.F.);
#3755=ORIENTED_EDGE('',*,*,#2828,.T.);
#3756=ORIENTED_EDGE('',*,*,#2829,.F.);
#3757=ORIENTED_EDGE('',*,*,#2830,.F.);
#3758=ORIENTED_EDGE('',*,*,#2828,.F.);
#3759=ORIENTED_EDGE('',*,*,#2831,.F.);
#3760=ORIENTED_EDGE('',*,*,#2832,.F.);
#3761=ORIENTED_EDGE('',*,*,#2825,.F.);
#3762=ORIENTED_EDGE('',*,*,#2833,.F.);
#3763=ORIENTED_EDGE('',*,*,#2831,.T.);
#3764=ORIENTED_EDGE('',*,*,#2827,.T.);
#3765=ORIENTED_EDGE('',*,*,#2834,.F.);
#3766=ORIENTED_EDGE('',*,*,#2835,.T.);
#3767=ORIENTED_EDGE('',*,*,#2836,.T.);
#3768=ORIENTED_EDGE('',*,*,#2835,.F.);
#3769=ORIENTED_EDGE('',*,*,#2832,.T.);
#3770=ORIENTED_EDGE('',*,*,#2833,.T.);
#3771=ORIENTED_EDGE('',*,*,#2826,.T.);
#3772=ORIENTED_EDGE('',*,*,#2824,.T.);
#3773=ORIENTED_EDGE('',*,*,#2837,.F.);
#3774=ORIENTED_EDGE('',*,*,#2838,.T.);
#3775=ORIENTED_EDGE('',*,*,#2839,.T.);
#3776=ORIENTED_EDGE('',*,*,#2838,.F.);
#3777=ORIENTED_EDGE('',*,*,#2829,.T.);
#3778=ORIENTED_EDGE('',*,*,#2830,.T.);
#3779=ORIENTED_EDGE('',*,*,#2837,.T.);
#3780=ORIENTED_EDGE('',*,*,#2834,.T.);
#3781=ORIENTED_EDGE('',*,*,#2839,.F.);
#3782=ORIENTED_EDGE('',*,*,#2836,.F.);
#3783=ORIENTED_EDGE('',*,*,#2840,.F.);
#3784=ORIENTED_EDGE('',*,*,#2841,.T.);
#3785=ORIENTED_EDGE('',*,*,#2842,.F.);
#3786=ORIENTED_EDGE('',*,*,#2843,.F.);
#3787=ORIENTED_EDGE('',*,*,#2844,.T.);
#3788=ORIENTED_EDGE('',*,*,#2845,.F.);
#3789=ORIENTED_EDGE('',*,*,#2846,.F.);
#3790=ORIENTED_EDGE('',*,*,#2844,.F.);
#3791=ORIENTED_EDGE('',*,*,#2847,.F.);
#3792=ORIENTED_EDGE('',*,*,#2848,.F.);
#3793=ORIENTED_EDGE('',*,*,#2841,.F.);
#3794=ORIENTED_EDGE('',*,*,#2849,.F.);
#3795=ORIENTED_EDGE('',*,*,#2847,.T.);
#3796=ORIENTED_EDGE('',*,*,#2843,.T.);
#3797=ORIENTED_EDGE('',*,*,#2850,.F.);
#3798=ORIENTED_EDGE('',*,*,#2851,.T.);
#3799=ORIENTED_EDGE('',*,*,#2852,.T.);
#3800=ORIENTED_EDGE('',*,*,#2851,.F.);
#3801=ORIENTED_EDGE('',*,*,#2848,.T.);
#3802=ORIENTED_EDGE('',*,*,#2849,.T.);
#3803=ORIENTED_EDGE('',*,*,#2842,.T.);
#3804=ORIENTED_EDGE('',*,*,#2840,.T.);
#3805=ORIENTED_EDGE('',*,*,#2853,.F.);
#3806=ORIENTED_EDGE('',*,*,#2854,.T.);
#3807=ORIENTED_EDGE('',*,*,#2855,.T.);
#3808=ORIENTED_EDGE('',*,*,#2854,.F.);
#3809=ORIENTED_EDGE('',*,*,#2845,.T.);
#3810=ORIENTED_EDGE('',*,*,#2846,.T.);
#3811=ORIENTED_EDGE('',*,*,#2853,.T.);
#3812=ORIENTED_EDGE('',*,*,#2850,.T.);
#3813=ORIENTED_EDGE('',*,*,#2855,.F.);
#3814=ORIENTED_EDGE('',*,*,#2852,.F.);
#3815=ORIENTED_EDGE('',*,*,#2856,.F.);
#3816=ORIENTED_EDGE('',*,*,#2857,.T.);
#3817=ORIENTED_EDGE('',*,*,#2858,.T.);
#3818=ORIENTED_EDGE('',*,*,#2857,.F.);
#3819=ORIENTED_EDGE('',*,*,#2859,.F.);
#3820=ORIENTED_EDGE('',*,*,#2860,.T.);
#3821=ORIENTED_EDGE('',*,*,#2861,.T.);
#3822=ORIENTED_EDGE('',*,*,#2860,.F.);
#3823=ORIENTED_EDGE('',*,*,#2859,.T.);
#3824=ORIENTED_EDGE('',*,*,#2856,.T.);
#3825=ORIENTED_EDGE('',*,*,#2861,.F.);
#3826=ORIENTED_EDGE('',*,*,#2858,.F.);
#3827=ORIENTED_EDGE('',*,*,#2862,.F.);
#3828=ORIENTED_EDGE('',*,*,#2863,.T.);
#3829=ORIENTED_EDGE('',*,*,#2864,.T.);
#3830=ORIENTED_EDGE('',*,*,#2863,.F.);
#3831=ORIENTED_EDGE('',*,*,#2865,.F.);
#3832=ORIENTED_EDGE('',*,*,#2866,.T.);
#3833=ORIENTED_EDGE('',*,*,#2867,.T.);
#3834=ORIENTED_EDGE('',*,*,#2866,.F.);
#3835=ORIENTED_EDGE('',*,*,#2865,.T.);
#3836=ORIENTED_EDGE('',*,*,#2862,.T.);
#3837=ORIENTED_EDGE('',*,*,#2867,.F.);
#3838=ORIENTED_EDGE('',*,*,#2864,.F.);
#3839=ORIENTED_EDGE('',*,*,#2868,.F.);
#3840=ORIENTED_EDGE('',*,*,#2869,.F.);
#3841=ORIENTED_EDGE('',*,*,#2870,.F.);
#3842=ORIENTED_EDGE('',*,*,#2871,.F.);
#3843=ORIENTED_EDGE('',*,*,#2872,.F.);
#3844=ORIENTED_EDGE('',*,*,#2873,.F.);
#3845=ORIENTED_EDGE('',*,*,#2874,.F.);
#3846=ORIENTED_EDGE('',*,*,#2875,.F.);
#3847=ORIENTED_EDGE('',*,*,#2872,.T.);
#3848=ORIENTED_EDGE('',*,*,#2876,.T.);
#3849=ORIENTED_EDGE('',*,*,#2877,.T.);
#3850=ORIENTED_EDGE('',*,*,#2878,.T.);
#3851=ORIENTED_EDGE('',*,*,#2871,.T.);
#3852=ORIENTED_EDGE('',*,*,#2879,.F.);
#3853=ORIENTED_EDGE('',*,*,#2880,.T.);
#3854=ORIENTED_EDGE('',*,*,#2876,.F.);
#3855=ORIENTED_EDGE('',*,*,#2870,.T.);
#3856=ORIENTED_EDGE('',*,*,#2881,.T.);
#3857=ORIENTED_EDGE('',*,*,#2882,.T.);
#3858=ORIENTED_EDGE('',*,*,#2879,.T.);
#3859=ORIENTED_EDGE('',*,*,#2869,.T.);
#3860=ORIENTED_EDGE('',*,*,#2883,.F.);
#3861=ORIENTED_EDGE('',*,*,#2884,.T.);
#3862=ORIENTED_EDGE('',*,*,#2881,.F.);
#3863=ORIENTED_EDGE('',*,*,#2885,.F.);
#3864=ORIENTED_EDGE('',*,*,#2886,.F.);
#3865=ORIENTED_EDGE('',*,*,#2877,.F.);
#3866=ORIENTED_EDGE('',*,*,#2880,.F.);
#3867=ORIENTED_EDGE('',*,*,#2882,.F.);
#3868=ORIENTED_EDGE('',*,*,#2884,.F.);
#3869=ORIENTED_EDGE('',*,*,#2887,.F.);
#3870=ORIENTED_EDGE('',*,*,#2888,.F.);
#3871=ORIENTED_EDGE('',*,*,#2873,.T.);
#3872=ORIENTED_EDGE('',*,*,#2878,.F.);
#3873=ORIENTED_EDGE('',*,*,#2886,.T.);
#3874=ORIENTED_EDGE('',*,*,#2889,.F.);
#3875=ORIENTED_EDGE('',*,*,#2868,.T.);
#3876=ORIENTED_EDGE('',*,*,#2890,.T.);
#3877=ORIENTED_EDGE('',*,*,#2887,.T.);
#3878=ORIENTED_EDGE('',*,*,#2883,.T.);
#3879=ORIENTED_EDGE('',*,*,#2874,.T.);
#3880=ORIENTED_EDGE('',*,*,#2889,.T.);
#3881=ORIENTED_EDGE('',*,*,#2885,.T.);
#3882=ORIENTED_EDGE('',*,*,#2891,.T.);
#3883=ORIENTED_EDGE('',*,*,#2875,.T.);
#3884=ORIENTED_EDGE('',*,*,#2891,.F.);
#3885=ORIENTED_EDGE('',*,*,#2888,.T.);
#3886=ORIENTED_EDGE('',*,*,#2890,.F.);
#3887=ORIENTED_EDGE('',*,*,#2892,.F.);
#3888=ORIENTED_EDGE('',*,*,#2893,.T.);
#3889=ORIENTED_EDGE('',*,*,#2894,.T.);
#3890=ORIENTED_EDGE('',*,*,#2895,.F.);
#3891=ORIENTED_EDGE('',*,*,#2896,.F.);
#3892=ORIENTED_EDGE('',*,*,#2897,.T.);
#3893=ORIENTED_EDGE('',*,*,#2898,.T.);
#3894=ORIENTED_EDGE('',*,*,#2893,.F.);
#3895=ORIENTED_EDGE('',*,*,#2899,.F.);
#3896=ORIENTED_EDGE('',*,*,#2900,.T.);
#3897=ORIENTED_EDGE('',*,*,#2901,.T.);
#3898=ORIENTED_EDGE('',*,*,#2897,.F.);
#3899=ORIENTED_EDGE('',*,*,#2902,.F.);
#3900=ORIENTED_EDGE('',*,*,#2903,.T.);
#3901=ORIENTED_EDGE('',*,*,#2904,.T.);
#3902=ORIENTED_EDGE('',*,*,#2900,.F.);
#3903=ORIENTED_EDGE('',*,*,#2905,.F.);
#3904=ORIENTED_EDGE('',*,*,#2906,.T.);
#3905=ORIENTED_EDGE('',*,*,#2907,.T.);
#3906=ORIENTED_EDGE('',*,*,#2903,.F.);
#3907=ORIENTED_EDGE('',*,*,#2908,.F.);
#3908=ORIENTED_EDGE('',*,*,#2895,.T.);
#3909=ORIENTED_EDGE('',*,*,#2909,.T.);
#3910=ORIENTED_EDGE('',*,*,#2906,.F.);
#3911=ORIENTED_EDGE('',*,*,#2909,.F.);
#3912=ORIENTED_EDGE('',*,*,#2894,.F.);
#3913=ORIENTED_EDGE('',*,*,#2898,.F.);
#3914=ORIENTED_EDGE('',*,*,#2901,.F.);
#3915=ORIENTED_EDGE('',*,*,#2904,.F.);
#3916=ORIENTED_EDGE('',*,*,#2907,.F.);
#3917=ORIENTED_EDGE('',*,*,#2910,.F.);
#3918=ORIENTED_EDGE('',*,*,#2892,.T.);
#3919=ORIENTED_EDGE('',*,*,#2908,.T.);
#3920=ORIENTED_EDGE('',*,*,#2905,.T.);
#3921=ORIENTED_EDGE('',*,*,#2902,.T.);
#3922=ORIENTED_EDGE('',*,*,#2899,.T.);
#3923=ORIENTED_EDGE('',*,*,#2896,.T.);
#3924=ORIENTED_EDGE('',*,*,#2911,.F.);
#3925=ORIENTED_EDGE('',*,*,#2912,.T.);
#3926=ORIENTED_EDGE('',*,*,#2910,.T.);
#3927=ORIENTED_EDGE('',*,*,#2912,.F.);
#3928=ORIENTED_EDGE('',*,*,#2913,.F.);
#3929=ORIENTED_EDGE('',*,*,#2914,.T.);
#3930=ORIENTED_EDGE('',*,*,#2911,.T.);
#3931=ORIENTED_EDGE('',*,*,#2914,.F.);
#3932=ORIENTED_EDGE('',*,*,#2915,.F.);
#3933=ORIENTED_EDGE('',*,*,#2916,.T.);
#3934=ORIENTED_EDGE('',*,*,#2913,.T.);
#3935=ORIENTED_EDGE('',*,*,#2916,.F.);
#3936=ORIENTED_EDGE('',*,*,#2915,.T.);
#3937=ORIENTED_EDGE('',*,*,#2917,.F.);
#3938=ORIENTED_EDGE('',*,*,#2918,.F.);
#3939=ORIENTED_EDGE('',*,*,#2919,.T.);
#3940=ORIENTED_EDGE('',*,*,#2917,.T.);
#3941=ORIENTED_EDGE('',*,*,#2919,.F.);
#3942=ORIENTED_EDGE('',*,*,#2920,.F.);
#3943=ORIENTED_EDGE('',*,*,#2921,.T.);
#3944=ORIENTED_EDGE('',*,*,#2918,.T.);
#3945=ORIENTED_EDGE('',*,*,#2921,.F.);
#3946=ORIENTED_EDGE('',*,*,#2922,.F.);
#3947=ORIENTED_EDGE('',*,*,#2923,.T.);
#3948=ORIENTED_EDGE('',*,*,#2920,.T.);
#3949=ORIENTED_EDGE('',*,*,#2923,.F.);
#3950=ORIENTED_EDGE('',*,*,#2922,.T.);
#3951=ORIENTED_EDGE('',*,*,#2924,.F.);
#3952=ORIENTED_EDGE('',*,*,#2925,.F.);
#3953=ORIENTED_EDGE('',*,*,#2926,.T.);
#3954=ORIENTED_EDGE('',*,*,#2924,.T.);
#3955=ORIENTED_EDGE('',*,*,#2926,.F.);
#3956=ORIENTED_EDGE('',*,*,#2927,.F.);
#3957=ORIENTED_EDGE('',*,*,#2928,.T.);
#3958=ORIENTED_EDGE('',*,*,#2925,.T.);
#3959=ORIENTED_EDGE('',*,*,#2928,.F.);
#3960=ORIENTED_EDGE('',*,*,#2929,.F.);
#3961=ORIENTED_EDGE('',*,*,#2930,.T.);
#3962=ORIENTED_EDGE('',*,*,#2927,.T.);
#3963=ORIENTED_EDGE('',*,*,#2930,.F.);
#3964=ORIENTED_EDGE('',*,*,#2929,.T.);
#3965=ORIENTED_EDGE('',*,*,#2931,.T.);
#3966=ORIENTED_EDGE('',*,*,#2932,.T.);
#3967=ORIENTED_EDGE('',*,*,#2933,.T.);
#3968=ORIENTED_EDGE('',*,*,#2934,.F.);
#3969=ORIENTED_EDGE('',*,*,#2935,.T.);
#3970=ORIENTED_EDGE('',*,*,#2936,.T.);
#3971=ORIENTED_EDGE('',*,*,#2937,.T.);
#3972=ORIENTED_EDGE('',*,*,#2932,.F.);
#3973=ORIENTED_EDGE('',*,*,#2938,.T.);
#3974=ORIENTED_EDGE('',*,*,#2939,.T.);
#3975=ORIENTED_EDGE('',*,*,#2940,.T.);
#3976=ORIENTED_EDGE('',*,*,#2936,.F.);
#3977=ORIENTED_EDGE('',*,*,#2941,.T.);
#3978=ORIENTED_EDGE('',*,*,#2942,.T.);
#3979=ORIENTED_EDGE('',*,*,#2943,.T.);
#3980=ORIENTED_EDGE('',*,*,#2939,.F.);
#3981=ORIENTED_EDGE('',*,*,#2944,.T.);
#3982=ORIENTED_EDGE('',*,*,#2945,.T.);
#3983=ORIENTED_EDGE('',*,*,#2946,.T.);
#3984=ORIENTED_EDGE('',*,*,#2942,.F.);
#3985=ORIENTED_EDGE('',*,*,#2947,.T.);
#3986=ORIENTED_EDGE('',*,*,#2934,.T.);
#3987=ORIENTED_EDGE('',*,*,#2948,.T.);
#3988=ORIENTED_EDGE('',*,*,#2945,.F.);
#3989=ORIENTED_EDGE('',*,*,#2947,.F.);
#3990=ORIENTED_EDGE('',*,*,#2944,.F.);
#3991=ORIENTED_EDGE('',*,*,#2941,.F.);
#3992=ORIENTED_EDGE('',*,*,#2938,.F.);
#3993=ORIENTED_EDGE('',*,*,#2935,.F.);
#3994=ORIENTED_EDGE('',*,*,#2931,.F.);
#3995=ORIENTED_EDGE('',*,*,#2948,.F.);
#3996=ORIENTED_EDGE('',*,*,#2933,.F.);
#3997=ORIENTED_EDGE('',*,*,#2937,.F.);
#3998=ORIENTED_EDGE('',*,*,#2940,.F.);
#3999=ORIENTED_EDGE('',*,*,#2943,.F.);
#4000=ORIENTED_EDGE('',*,*,#2946,.F.);
#4001=CYLINDRICAL_SURFACE('',#4656,0.33);
#4002=CYLINDRICAL_SURFACE('',#4659,0.33);
#4003=CYLINDRICAL_SURFACE('',#4662,0.33);
#4004=CYLINDRICAL_SURFACE('',#4665,0.33);
#4005=CYLINDRICAL_SURFACE('',#4668,0.34);
#4006=CYLINDRICAL_SURFACE('',#4671,0.34);
#4007=CYLINDRICAL_SURFACE('',#4674,0.34);
#4008=CYLINDRICAL_SURFACE('',#4677,0.34);
#4009=CYLINDRICAL_SURFACE('',#4680,0.34);
#4010=CYLINDRICAL_SURFACE('',#4683,0.34);
#4011=CYLINDRICAL_SURFACE('',#4693,0.25);
#4012=CYLINDRICAL_SURFACE('',#4697,0.25);
#4013=CYLINDRICAL_SURFACE('',#4715,0.25);
#4014=CYLINDRICAL_SURFACE('',#4719,0.25);
#4015=CYLINDRICAL_SURFACE('',#4737,0.425);
#4016=CYLINDRICAL_SURFACE('',#4740,0.645);
#4017=CYLINDRICAL_SURFACE('',#4746,0.425);
#4018=CYLINDRICAL_SURFACE('',#4749,0.645);
#4019=CYLINDRICAL_SURFACE('',#4755,0.425);
#4020=CYLINDRICAL_SURFACE('',#4758,0.645);
#4021=CYLINDRICAL_SURFACE('',#4764,0.425);
#4022=CYLINDRICAL_SURFACE('',#4767,0.645);
#4023=CYLINDRICAL_SURFACE('',#4773,0.425);
#4024=CYLINDRICAL_SURFACE('',#4776,0.645);
#4025=CYLINDRICAL_SURFACE('',#4782,0.425);
#4026=CYLINDRICAL_SURFACE('',#4785,0.645);
#4027=CYLINDRICAL_SURFACE('',#4791,0.32);
#4028=CYLINDRICAL_SURFACE('',#4794,0.6);
#4029=CYLINDRICAL_SURFACE('',#4804,0.5);
#4030=CYLINDRICAL_SURFACE('',#4812,0.2942);
#4031=CYLINDRICAL_SURFACE('',#4827,2.05);
#4032=CYLINDRICAL_SURFACE('',#4830,2.05);
#4033=CYLINDRICAL_SURFACE('',#4848,2.8);
#4034=CYLINDRICAL_SURFACE('',#4858,0.65);
#4035=CYLINDRICAL_SURFACE('',#4860,0.65);
#4036=CYLINDRICAL_SURFACE('',#4868,1.8);
#4037=CYLINDRICAL_SURFACE('',#4877,0.25);
#4038=CYLINDRICAL_SURFACE('',#4878,0.25);
#4039=CYLINDRICAL_SURFACE('',#4879,1.65);
#4040=CYLINDRICAL_SURFACE('',#4882,0.25);
#4041=CYLINDRICAL_SURFACE('',#4883,0.25);
#4042=CYLINDRICAL_SURFACE('',#4884,0.25);
#4043=CYLINDRICAL_SURFACE('',#4885,0.25);
#4044=CYLINDRICAL_SURFACE('',#4890,1.75);
#4045=CYLINDRICAL_SURFACE('',#4894,1.);
#4046=CYLINDRICAL_SURFACE('',#4898,0.42);
#4047=CYLINDRICAL_SURFACE('',#4901,0.8);
#4048=CYLINDRICAL_SURFACE('',#4921,0.65);
#4049=CYLINDRICAL_SURFACE('',#4929,0.3933);
#4050=CYLINDRICAL_SURFACE('',#4966,0.21);
#4051=CYLINDRICAL_SURFACE('',#4970,0.21);
#4052=CYLINDRICAL_SURFACE('',#4988,1.);
#4053=CYLINDRICAL_SURFACE('',#4996,0.21);
#4054=CYLINDRICAL_SURFACE('',#5006,1.);
#4055=CYLINDRICAL_SURFACE('',#5008,2.);
#4056=CYLINDRICAL_SURFACE('',#5014,0.21);
#4057=CYLINDRICAL_SURFACE('',#5024,1.);
#4058=CYLINDRICAL_SURFACE('',#5026,2.);
#4059=CYLINDRICAL_SURFACE('',#5032,0.21);
#4060=CYLINDRICAL_SURFACE('',#5036,1.005);
#4061=CYLINDRICAL_SURFACE('',#5039,1.5);
#4062=CYLINDRICAL_SURFACE('',#5047,0.21);
#4063=CYLINDRICAL_SURFACE('',#5051,1.005);
#4064=CYLINDRICAL_SURFACE('',#5054,1.5);
#4065=CYLINDRICAL_SURFACE('',#5060,0.275);
#4066=CYLINDRICAL_SURFACE('',#5063,1.1);
#4067=CYLINDRICAL_SURFACE('',#5069,0.275);
#4068=CYLINDRICAL_SURFACE('',#5072,1.1);
#4069=CYLINDRICAL_SURFACE('',#5100,0.24505);
#4070=CYLINDRICAL_SURFACE('',#5110,0.425);
#4071=CYLINDRICAL_SURFACE('',#5118,0.24505);
#4072=ADVANCED_FACE('',(#654),#4001,.F.);
#4073=ADVANCED_FACE('',(#655),#4002,.F.);
#4074=ADVANCED_FACE('',(#656),#4003,.F.);
#4075=ADVANCED_FACE('',(#657),#4004,.F.);
#4076=ADVANCED_FACE('',(#658),#4005,.F.);
#4077=ADVANCED_FACE('',(#659),#4006,.F.);
#4078=ADVANCED_FACE('',(#660),#4007,.F.);
#4079=ADVANCED_FACE('',(#661),#4008,.F.);
#4080=ADVANCED_FACE('',(#662),#4009,.F.);
#4081=ADVANCED_FACE('',(#663),#4010,.F.);
#4082=ADVANCED_FACE('',(#664),#488,.T.);
#4083=ADVANCED_FACE('',(#665),#489,.T.);
#4084=ADVANCED_FACE('',(#666),#490,.T.);
#4085=ADVANCED_FACE('',(#667),#491,.T.);
#4086=ADVANCED_FACE('',(#668,#391,#392,#393,#394,#395,#396,#397,#398,#399,
#400),#492,.T.);
#4087=ADVANCED_FACE('',(#669,#401,#402,#403,#404,#405,#406,#407,#408,#409,
#410),#493,.F.);
#4088=ADVANCED_FACE('',(#670),#4011,.F.);
#4089=ADVANCED_FACE('',(#671),#494,.T.);
#4090=ADVANCED_FACE('',(#672),#4012,.F.);
#4091=ADVANCED_FACE('',(#673),#495,.T.);
#4092=ADVANCED_FACE('',(#674),#496,.T.);
#4093=ADVANCED_FACE('',(#675),#497,.T.);
#4094=ADVANCED_FACE('',(#676),#498,.T.);
#4095=ADVANCED_FACE('',(#677),#499,.T.);
#4096=ADVANCED_FACE('',(#678,#411,#412),#500,.T.);
#4097=ADVANCED_FACE('',(#679),#501,.F.);
#4098=ADVANCED_FACE('',(#680),#502,.T.);
#4099=ADVANCED_FACE('',(#681),#503,.T.);
#4100=ADVANCED_FACE('',(#682),#504,.T.);
#4101=ADVANCED_FACE('',(#683),#505,.T.);
#4102=ADVANCED_FACE('',(#684),#506,.T.);
#4103=ADVANCED_FACE('',(#685),#507,.F.);
#4104=ADVANCED_FACE('',(#686),#4013,.F.);
#4105=ADVANCED_FACE('',(#687),#508,.T.);
#4106=ADVANCED_FACE('',(#688),#4014,.F.);
#4107=ADVANCED_FACE('',(#689),#509,.T.);
#4108=ADVANCED_FACE('',(#690),#510,.T.);
#4109=ADVANCED_FACE('',(#691),#511,.T.);
#4110=ADVANCED_FACE('',(#692),#512,.T.);
#4111=ADVANCED_FACE('',(#693),#513,.T.);
#4112=ADVANCED_FACE('',(#694,#413,#414),#514,.T.);
#4113=ADVANCED_FACE('',(#695),#515,.F.);
#4114=ADVANCED_FACE('',(#696),#516,.T.);
#4115=ADVANCED_FACE('',(#697),#517,.T.);
#4116=ADVANCED_FACE('',(#698),#518,.T.);
#4117=ADVANCED_FACE('',(#699),#519,.T.);
#4118=ADVANCED_FACE('',(#700),#520,.T.);
#4119=ADVANCED_FACE('',(#701),#521,.F.);
#4120=ADVANCED_FACE('',(#702),#4015,.F.);
#4121=ADVANCED_FACE('',(#703),#4016,.T.);
#4122=ADVANCED_FACE('',(#704,#415),#522,.T.);
#4123=ADVANCED_FACE('',(#705,#416),#523,.F.);
#4124=ADVANCED_FACE('',(#706),#4017,.F.);
#4125=ADVANCED_FACE('',(#707),#4018,.T.);
#4126=ADVANCED_FACE('',(#708,#417),#524,.T.);
#4127=ADVANCED_FACE('',(#709,#418),#525,.F.);
#4128=ADVANCED_FACE('',(#710),#4019,.F.);
#4129=ADVANCED_FACE('',(#711),#4020,.T.);
#4130=ADVANCED_FACE('',(#712,#419),#526,.T.);
#4131=ADVANCED_FACE('',(#713,#420),#527,.F.);
#4132=ADVANCED_FACE('',(#714),#4021,.F.);
#4133=ADVANCED_FACE('',(#715),#4022,.T.);
#4134=ADVANCED_FACE('',(#716,#421),#528,.T.);
#4135=ADVANCED_FACE('',(#717,#422),#529,.F.);
#4136=ADVANCED_FACE('',(#718),#4023,.F.);
#4137=ADVANCED_FACE('',(#719),#4024,.T.);
#4138=ADVANCED_FACE('',(#720,#423),#530,.T.);
#4139=ADVANCED_FACE('',(#721,#424),#531,.F.);
#4140=ADVANCED_FACE('',(#722),#4025,.F.);
#4141=ADVANCED_FACE('',(#723),#4026,.T.);
#4142=ADVANCED_FACE('',(#724,#425),#532,.T.);
#4143=ADVANCED_FACE('',(#725,#426),#533,.F.);
#4144=ADVANCED_FACE('',(#726),#4027,.F.);
#4145=ADVANCED_FACE('',(#727),#4028,.T.);
#4146=ADVANCED_FACE('',(#728,#427),#534,.T.);
#4147=ADVANCED_FACE('',(#729,#428),#535,.F.);
#4148=ADVANCED_FACE('',(#730),#536,.T.);
#4149=ADVANCED_FACE('',(#731),#268,.T.);
#4150=ADVANCED_FACE('',(#732),#4029,.T.);
#4151=ADVANCED_FACE('',(#733),#269,.T.);
#4152=ADVANCED_FACE('',(#734,#429),#537,.T.);
#4153=ADVANCED_FACE('',(#735),#270,.T.);
#4154=ADVANCED_FACE('',(#736),#4030,.T.);
#4155=ADVANCED_FACE('',(#737),#271,.T.);
#4156=ADVANCED_FACE('',(#738),#538,.T.);
#4157=ADVANCED_FACE('',(#739),#539,.F.);
#4158=ADVANCED_FACE('',(#740),#540,.F.);
#4159=ADVANCED_FACE('',(#741),#541,.F.);
#4160=ADVANCED_FACE('',(#742),#542,.F.);
#4161=ADVANCED_FACE('',(#743),#543,.F.);
#4162=ADVANCED_FACE('',(#744),#544,.F.);
#4163=ADVANCED_FACE('',(#745),#545,.F.);
#4164=ADVANCED_FACE('',(#746),#546,.F.);
#4165=ADVANCED_FACE('',(#747),#4031,.F.);
#4166=ADVANCED_FACE('',(#748),#4032,.F.);
#4167=ADVANCED_FACE('',(#749,#430,#431),#263,.F.);
#4168=ADVANCED_FACE('',(#750),#547,.T.);
#4169=ADVANCED_FACE('',(#751),#548,.T.);
#4170=ADVANCED_FACE('',(#752),#549,.T.);
#4171=ADVANCED_FACE('',(#753),#550,.T.);
#4172=ADVANCED_FACE('',(#754),#551,.T.);
#4173=ADVANCED_FACE('',(#755),#552,.T.);
#4174=ADVANCED_FACE('',(#756,#432,#433,#434),#553,.T.);
#4175=ADVANCED_FACE('',(#757),#4033,.T.);
#4176=ADVANCED_FACE('',(#758,#435),#554,.F.);
#4177=ADVANCED_FACE('',(#759,#436),#555,.T.);
#4178=ADVANCED_FACE('',(#760),#556,.F.);
#4179=ADVANCED_FACE('',(#761),#557,.F.);
#4180=ADVANCED_FACE('',(#762),#558,.F.);
#4181=ADVANCED_FACE('',(#763),#559,.F.);
#4182=ADVANCED_FACE('',(#764),#560,.F.);
#4183=ADVANCED_FACE('',(#765),#4034,.F.);
#4184=ADVANCED_FACE('',(#766),#4035,.F.);
#4185=ADVANCED_FACE('',(#767),#561,.T.);
#4186=ADVANCED_FACE('',(#768),#562,.T.);
#4187=ADVANCED_FACE('',(#769),#563,.T.);
#4188=ADVANCED_FACE('',(#770),#564,.T.);
#4189=ADVANCED_FACE('',(#771,#437,#438,#439),#565,.F.);
#4190=ADVANCED_FACE('',(#772),#4036,.F.);
#4191=ADVANCED_FACE('',(#773,#440),#566,.T.);
#4192=ADVANCED_FACE('',(#774,#441,#442),#264,.T.);
#4193=ADVANCED_FACE('',(#775,#443),#567,.T.);
#4194=ADVANCED_FACE('',(#776),#4037,.F.);
#4195=ADVANCED_FACE('',(#777),#4038,.F.);
#4196=ADVANCED_FACE('',(#778,#444,#445,#446,#447,#448,#449),#4039,.T.);
#4197=ADVANCED_FACE('',(#779),#4040,.F.);
#4198=ADVANCED_FACE('',(#780),#4041,.F.);
#4199=ADVANCED_FACE('',(#781),#4042,.F.);
#4200=ADVANCED_FACE('',(#782),#4043,.F.);
#4201=ADVANCED_FACE('',(#783,#450),#568,.T.);
#4202=ADVANCED_FACE('',(#784,#451),#569,.T.);
#4203=ADVANCED_FACE('',(#785),#4044,.T.);
#4204=ADVANCED_FACE('',(#786,#452),#570,.T.);
#4205=ADVANCED_FACE('',(#787,#453,#454,#455,#456,#457,#458),#4045,.F.);
#4206=ADVANCED_FACE('',(#788),#4046,.F.);
#4207=ADVANCED_FACE('',(#789),#4047,.T.);
#4208=ADVANCED_FACE('',(#790,#459),#571,.T.);
#4209=ADVANCED_FACE('',(#791,#460),#572,.F.);
#4210=ADVANCED_FACE('',(#792),#573,.F.);
#4211=ADVANCED_FACE('',(#793),#574,.F.);
#4212=ADVANCED_FACE('',(#794),#575,.F.);
#4213=ADVANCED_FACE('',(#795),#576,.F.);
#4214=ADVANCED_FACE('',(#796),#577,.F.);
#4215=ADVANCED_FACE('',(#797),#578,.F.);
#4216=ADVANCED_FACE('',(#798),#579,.F.);
#4217=ADVANCED_FACE('',(#799),#580,.F.);
#4218=ADVANCED_FACE('',(#800),#581,.F.);
#4219=ADVANCED_FACE('',(#801),#582,.T.);
#4220=ADVANCED_FACE('',(#802),#272,.T.);
#4221=ADVANCED_FACE('',(#803),#4048,.T.);
#4222=ADVANCED_FACE('',(#804),#273,.T.);
#4223=ADVANCED_FACE('',(#805,#461),#583,.T.);
#4224=ADVANCED_FACE('',(#806),#274,.T.);
#4225=ADVANCED_FACE('',(#807),#4049,.T.);
#4226=ADVANCED_FACE('',(#808),#4050,.F.);
#4227=ADVANCED_FACE('',(#809),#584,.T.);
#4228=ADVANCED_FACE('',(#810),#4051,.F.);
#4229=ADVANCED_FACE('',(#811),#585,.F.);
#4230=ADVANCED_FACE('',(#812),#586,.F.);
#4231=ADVANCED_FACE('',(#813),#587,.T.);
#4232=ADVANCED_FACE('',(#814),#588,.F.);
#4233=ADVANCED_FACE('',(#815),#589,.F.);
#4234=ADVANCED_FACE('',(#816),#590,.F.);
#4235=ADVANCED_FACE('',(#817),#591,.F.);
#4236=ADVANCED_FACE('',(#818),#592,.T.);
#4237=ADVANCED_FACE('',(#819),#593,.F.);
#4238=ADVANCED_FACE('',(#820),#594,.F.);
#4239=ADVANCED_FACE('',(#821),#595,.F.);
#4240=ADVANCED_FACE('',(#822,#462,#463),#4052,.T.);
#4241=ADVANCED_FACE('',(#823,#464),#596,.T.);
#4242=ADVANCED_FACE('',(#824,#465),#597,.F.);
#4243=ADVANCED_FACE('',(#825),#598,.T.);
#4244=ADVANCED_FACE('',(#826),#4053,.F.);
#4245=ADVANCED_FACE('',(#827),#599,.T.);
#4246=ADVANCED_FACE('',(#828),#600,.F.);
#4247=ADVANCED_FACE('',(#829),#601,.F.);
#4248=ADVANCED_FACE('',(#830),#602,.F.);
#4249=ADVANCED_FACE('',(#831,#466),#603,.T.);
#4250=ADVANCED_FACE('',(#832,#467),#4054,.F.);
#4251=ADVANCED_FACE('',(#833,#468),#4055,.T.);
#4252=ADVANCED_FACE('',(#834,#469),#604,.F.);
#4253=ADVANCED_FACE('',(#835),#605,.T.);
#4254=ADVANCED_FACE('',(#836),#4056,.F.);
#4255=ADVANCED_FACE('',(#837),#606,.T.);
#4256=ADVANCED_FACE('',(#838),#607,.F.);
#4257=ADVANCED_FACE('',(#839),#608,.F.);
#4258=ADVANCED_FACE('',(#840),#609,.F.);
#4259=ADVANCED_FACE('',(#841,#470),#610,.T.);
#4260=ADVANCED_FACE('',(#842,#471),#4057,.F.);
#4261=ADVANCED_FACE('',(#843,#472),#4058,.T.);
#4262=ADVANCED_FACE('',(#844,#473),#611,.F.);
#4263=ADVANCED_FACE('',(#845),#612,.T.);
#4264=ADVANCED_FACE('',(#846),#4059,.F.);
#4265=ADVANCED_FACE('',(#847),#613,.T.);
#4266=ADVANCED_FACE('',(#848,#474),#4060,.F.);
#4267=ADVANCED_FACE('',(#849,#475),#4061,.T.);
#4268=ADVANCED_FACE('',(#850,#476),#614,.T.);
#4269=ADVANCED_FACE('',(#851,#477),#615,.F.);
#4270=ADVANCED_FACE('',(#852),#616,.T.);
#4271=ADVANCED_FACE('',(#853),#4062,.F.);
#4272=ADVANCED_FACE('',(#854),#617,.T.);
#4273=ADVANCED_FACE('',(#855,#478),#4063,.F.);
#4274=ADVANCED_FACE('',(#856,#479),#4064,.T.);
#4275=ADVANCED_FACE('',(#857,#480),#618,.T.);
#4276=ADVANCED_FACE('',(#858,#481),#619,.F.);
#4277=ADVANCED_FACE('',(#859),#4065,.F.);
#4278=ADVANCED_FACE('',(#860),#4066,.T.);
#4279=ADVANCED_FACE('',(#861,#482),#620,.T.);
#4280=ADVANCED_FACE('',(#862,#483),#621,.F.);
#4281=ADVANCED_FACE('',(#863),#4067,.F.);
#4282=ADVANCED_FACE('',(#864),#4068,.T.);
#4283=ADVANCED_FACE('',(#865,#484),#622,.T.);
#4284=ADVANCED_FACE('',(#866,#485),#623,.F.);
#4285=ADVANCED_FACE('',(#867),#624,.F.);
#4286=ADVANCED_FACE('',(#868),#625,.T.);
#4287=ADVANCED_FACE('',(#869),#626,.T.);
#4288=ADVANCED_FACE('',(#870),#627,.T.);
#4289=ADVANCED_FACE('',(#871),#628,.T.);
#4290=ADVANCED_FACE('',(#872),#629,.T.);
#4291=ADVANCED_FACE('',(#873),#630,.F.);
#4292=ADVANCED_FACE('',(#874),#631,.T.);
#4293=ADVANCED_FACE('',(#875),#632,.T.);
#4294=ADVANCED_FACE('',(#876),#633,.T.);
#4295=ADVANCED_FACE('',(#877),#634,.F.);
#4296=ADVANCED_FACE('',(#878),#635,.F.);
#4297=ADVANCED_FACE('',(#879),#636,.F.);
#4298=ADVANCED_FACE('',(#880),#637,.F.);
#4299=ADVANCED_FACE('',(#881),#638,.F.);
#4300=ADVANCED_FACE('',(#882),#639,.F.);
#4301=ADVANCED_FACE('',(#883),#640,.F.);
#4302=ADVANCED_FACE('',(#884,#486),#641,.T.);
#4303=ADVANCED_FACE('',(#885),#275,.T.);
#4304=ADVANCED_FACE('',(#886),#4069,.T.);
#4305=ADVANCED_FACE('',(#887),#276,.T.);
#4306=ADVANCED_FACE('',(#888),#642,.T.);
#4307=ADVANCED_FACE('',(#889),#643,.T.);
#4308=ADVANCED_FACE('',(#890),#277,.T.);
#4309=ADVANCED_FACE('',(#891),#4070,.T.);
#4310=ADVANCED_FACE('',(#892),#278,.T.);
#4311=ADVANCED_FACE('',(#893,#487),#644,.T.);
#4312=ADVANCED_FACE('',(#894),#279,.T.);
#4313=ADVANCED_FACE('',(#895),#4071,.T.);
#4314=ADVANCED_FACE('',(#896),#280,.T.);
#4315=ADVANCED_FACE('',(#897),#645,.T.);
#4316=ADVANCED_FACE('',(#898),#646,.F.);
#4317=ADVANCED_FACE('',(#899),#647,.F.);
#4318=ADVANCED_FACE('',(#900),#648,.F.);
#4319=ADVANCED_FACE('',(#901),#649,.F.);
#4320=ADVANCED_FACE('',(#902),#650,.F.);
#4321=ADVANCED_FACE('',(#903),#651,.F.);
#4322=ADVANCED_FACE('',(#904),#652,.F.);
#4323=ADVANCED_FACE('',(#905),#653,.F.);
#4324=CLOSED_SHELL('',(#4072,#4073,#4074,#4075,#4076,#4077,#4078,#4079,
#4080,#4081,#4082,#4083,#4084,#4085,#4086,#4087));
#4325=CLOSED_SHELL('',(#4088,#4089,#4090,#4091,#4092,#4093,#4094,#4095,
#4096,#4097));
#4326=CLOSED_SHELL('',(#4098,#4099,#4100,#4101,#4102,#4103));
#4327=CLOSED_SHELL('',(#4104,#4105,#4106,#4107,#4108,#4109,#4110,#4111,
#4112,#4113));
#4328=CLOSED_SHELL('',(#4114,#4115,#4116,#4117,#4118,#4119));
#4329=CLOSED_SHELL('',(#4120,#4121,#4122,#4123));
#4330=CLOSED_SHELL('',(#4124,#4125,#4126,#4127));
#4331=CLOSED_SHELL('',(#4128,#4129,#4130,#4131));
#4332=CLOSED_SHELL('',(#4132,#4133,#4134,#4135));
#4333=CLOSED_SHELL('',(#4136,#4137,#4138,#4139));
#4334=CLOSED_SHELL('',(#4140,#4141,#4142,#4143));
#4335=CLOSED_SHELL('',(#4144,#4145,#4146,#4147));
#4336=CLOSED_SHELL('',(#4148,#4149,#4150,#4151,#4152,#4153,#4154,#4155,
#4156));
#4337=CLOSED_SHELL('',(#4157,#4158,#4159,#4160,#4161,#4162,#4163,#4164));
#4338=CLOSED_SHELL('',(#4165,#4166,#4167,#4168,#4169,#4170,#4171,#4172,
#4173,#4174,#4175,#4176,#4177,#4178,#4179,#4180,#4181,#4182,#4183,#4184,
#4185,#4186,#4187,#4188,#4189));
#4339=CLOSED_SHELL('',(#4190,#4191,#4192,#4193));
#4340=CLOSED_SHELL('',(#4194,#4195,#4196,#4197,#4198,#4199,#4200,#4201,
#4202,#4203,#4204,#4205));
#4341=CLOSED_SHELL('',(#4206,#4207,#4208,#4209));
#4342=CLOSED_SHELL('',(#4210,#4211,#4212,#4213,#4214,#4215,#4216,#4217));
#4343=CLOSED_SHELL('',(#4218,#4219,#4220,#4221,#4222,#4223,#4224,#4225));
#4344=CLOSED_SHELL('',(#4226,#4227,#4228,#4229,#4230,#4231,#4232,#4233,
#4234,#4235,#4236,#4237,#4238,#4239,#4240,#4241,#4242));
#4345=CLOSED_SHELL('',(#4243,#4244,#4245,#4246,#4247,#4248,#4249,#4250,
#4251,#4252));
#4346=CLOSED_SHELL('',(#4253,#4254,#4255,#4256,#4257,#4258,#4259,#4260,
#4261,#4262));
#4347=CLOSED_SHELL('',(#4263,#4264,#4265,#4266,#4267,#4268,#4269));
#4348=CLOSED_SHELL('',(#4270,#4271,#4272,#4273,#4274,#4275,#4276));
#4349=CLOSED_SHELL('',(#4277,#4278,#4279,#4280));
#4350=CLOSED_SHELL('',(#4281,#4282,#4283,#4284));
#4351=CLOSED_SHELL('',(#4285,#4286,#4287,#4288,#4289,#4290,#4291,#4292,
#4293,#4294));
#4352=CLOSED_SHELL('',(#4295,#4296,#4297,#4298,#4299,#4300,#4301,#4302,
#4303,#4304,#4305,#4306));
#4353=CLOSED_SHELL('',(#4307,#4308,#4309,#4310,#4311,#4312,#4313,#4314,
#4315));
#4354=CLOSED_SHELL('',(#4316,#4317,#4318,#4319,#4320,#4321,#4322,#4323));
#4355=DERIVED_UNIT_ELEMENT(#4409,1.);
#4356=DERIVED_UNIT_ELEMENT(#8379,-3.);
#4357=DERIVED_UNIT_ELEMENT(#4409,1.);
#4358=DERIVED_UNIT_ELEMENT(#8379,-3.);
#4359=DERIVED_UNIT_ELEMENT(#4409,1.);
#4360=DERIVED_UNIT_ELEMENT(#8379,-3.);
#4361=DERIVED_UNIT_ELEMENT(#4409,1.);
#4362=DERIVED_UNIT_ELEMENT(#8379,-3.);
#4363=DERIVED_UNIT_ELEMENT(#4409,1.);
#4364=DERIVED_UNIT_ELEMENT(#8379,-3.);
#4365=DERIVED_UNIT_ELEMENT(#4409,1.);
#4366=DERIVED_UNIT_ELEMENT(#8379,-3.);
#4367=DERIVED_UNIT_ELEMENT(#4409,1.);
#4368=DERIVED_UNIT_ELEMENT(#8379,-3.);
#4369=DERIVED_UNIT_ELEMENT(#4409,1.);
#4370=DERIVED_UNIT_ELEMENT(#8379,-3.);
#4371=DERIVED_UNIT_ELEMENT(#4409,1.);
#4372=DERIVED_UNIT_ELEMENT(#8379,-3.);
#4373=DERIVED_UNIT_ELEMENT(#4409,1.);
#4374=DERIVED_UNIT_ELEMENT(#8379,-3.);
#4375=DERIVED_UNIT_ELEMENT(#4409,1.);
#4376=DERIVED_UNIT_ELEMENT(#8379,-3.);
#4377=DERIVED_UNIT_ELEMENT(#4409,1.);
#4378=DERIVED_UNIT_ELEMENT(#8379,-3.);
#4379=DERIVED_UNIT_ELEMENT(#4409,1.);
#4380=DERIVED_UNIT_ELEMENT(#8379,-3.);
#4381=DERIVED_UNIT_ELEMENT(#4409,1.);
#4382=DERIVED_UNIT_ELEMENT(#8379,-3.);
#4383=DERIVED_UNIT_ELEMENT(#4409,1.);
#4384=DERIVED_UNIT_ELEMENT(#8379,-3.);
#4385=DERIVED_UNIT_ELEMENT(#4409,1.);
#4386=DERIVED_UNIT_ELEMENT(#8379,-3.);
#4387=DERIVED_UNIT_ELEMENT(#4409,1.);
#4388=DERIVED_UNIT_ELEMENT(#8379,-3.);
#4389=DERIVED_UNIT_ELEMENT(#4409,1.);
#4390=DERIVED_UNIT_ELEMENT(#8379,-3.);
#4391=DERIVED_UNIT_ELEMENT(#4409,1.);
#4392=DERIVED_UNIT_ELEMENT(#8379,-3.);
#4393=DERIVED_UNIT_ELEMENT(#4409,1.);
#4394=DERIVED_UNIT_ELEMENT(#8379,-3.);
#4395=DERIVED_UNIT_ELEMENT(#4409,1.);
#4396=DERIVED_UNIT_ELEMENT(#8379,-3.);
#4397=DERIVED_UNIT_ELEMENT(#4409,1.);
#4398=DERIVED_UNIT_ELEMENT(#8379,-3.);
#4399=DERIVED_UNIT_ELEMENT(#4409,1.);
#4400=DERIVED_UNIT_ELEMENT(#8379,-3.);
#4401=DERIVED_UNIT_ELEMENT(#4409,1.);
#4402=DERIVED_UNIT_ELEMENT(#8379,-3.);
#4403=DERIVED_UNIT_ELEMENT(#4409,1.);
#4404=DERIVED_UNIT_ELEMENT(#8379,-3.);
#4405=DERIVED_UNIT_ELEMENT(#4409,1.);
#4406=DERIVED_UNIT_ELEMENT(#8379,-3.);
#4407=DERIVED_UNIT_ELEMENT(#4409,1.);
#4408=DERIVED_UNIT_ELEMENT(#8379,-3.);
#4409=(
MASS_UNIT()
NAMED_UNIT(*)
SI_UNIT(.KILO.,.GRAM.)
);
#4410=DERIVED_UNIT((#4355,#4356));
#4411=DERIVED_UNIT((#4357,#4358));
#4412=DERIVED_UNIT((#4359,#4360));
#4413=DERIVED_UNIT((#4361,#4362));
#4414=DERIVED_UNIT((#4363,#4364));
#4415=DERIVED_UNIT((#4365,#4366));
#4416=DERIVED_UNIT((#4367,#4368));
#4417=DERIVED_UNIT((#4369,#4370));
#4418=DERIVED_UNIT((#4371,#4372));
#4419=DERIVED_UNIT((#4373,#4374));
#4420=DERIVED_UNIT((#4375,#4376));
#4421=DERIVED_UNIT((#4377,#4378));
#4422=DERIVED_UNIT((#4379,#4380));
#4423=DERIVED_UNIT((#4381,#4382));
#4424=DERIVED_UNIT((#4383,#4384));
#4425=DERIVED_UNIT((#4385,#4386));
#4426=DERIVED_UNIT((#4387,#4388));
#4427=DERIVED_UNIT((#4389,#4390));
#4428=DERIVED_UNIT((#4391,#4392));
#4429=DERIVED_UNIT((#4393,#4394));
#4430=DERIVED_UNIT((#4395,#4396));
#4431=DERIVED_UNIT((#4397,#4398));
#4432=DERIVED_UNIT((#4399,#4400));
#4433=DERIVED_UNIT((#4401,#4402));
#4434=DERIVED_UNIT((#4403,#4404));
#4435=DERIVED_UNIT((#4405,#4406));
#4436=DERIVED_UNIT((#4407,#4408));
#4437=MEASURE_REPRESENTATION_ITEM('density measure',
POSITIVE_RATIO_MEASURE(7850.),#4410);
#4438=MEASURE_REPRESENTATION_ITEM('density measure',
POSITIVE_RATIO_MEASURE(7850.),#4411);
#4439=MEASURE_REPRESENTATION_ITEM('density measure',
POSITIVE_RATIO_MEASURE(7850.),#4412);
#4440=MEASURE_REPRESENTATION_ITEM('density measure',
POSITIVE_RATIO_MEASURE(7850.),#4413);
#4441=MEASURE_REPRESENTATION_ITEM('density measure',
POSITIVE_RATIO_MEASURE(7850.),#4414);
#4442=MEASURE_REPRESENTATION_ITEM('density measure',
POSITIVE_RATIO_MEASURE(7850.),#4415);
#4443=MEASURE_REPRESENTATION_ITEM('density measure',
POSITIVE_RATIO_MEASURE(7850.),#4416);
#4444=MEASURE_REPRESENTATION_ITEM('density measure',
POSITIVE_RATIO_MEASURE(7850.),#4417);
#4445=MEASURE_REPRESENTATION_ITEM('density measure',
POSITIVE_RATIO_MEASURE(7850.),#4418);
#4446=MEASURE_REPRESENTATION_ITEM('density measure',
POSITIVE_RATIO_MEASURE(7850.),#4419);
#4447=MEASURE_REPRESENTATION_ITEM('density measure',
POSITIVE_RATIO_MEASURE(7850.),#4420);
#4448=MEASURE_REPRESENTATION_ITEM('density measure',
POSITIVE_RATIO_MEASURE(7850.),#4421);
#4449=MEASURE_REPRESENTATION_ITEM('density measure',
POSITIVE_RATIO_MEASURE(7850.),#4422);
#4450=MEASURE_REPRESENTATION_ITEM('density measure',
POSITIVE_RATIO_MEASURE(7850.),#4423);
#4451=MEASURE_REPRESENTATION_ITEM('density measure',
POSITIVE_RATIO_MEASURE(7850.),#4424);
#4452=MEASURE_REPRESENTATION_ITEM('density measure',
POSITIVE_RATIO_MEASURE(7850.),#4425);
#4453=MEASURE_REPRESENTATION_ITEM('density measure',
POSITIVE_RATIO_MEASURE(7850.),#4426);
#4454=MEASURE_REPRESENTATION_ITEM('density measure',
POSITIVE_RATIO_MEASURE(7850.),#4427);
#4455=MEASURE_REPRESENTATION_ITEM('density measure',
POSITIVE_RATIO_MEASURE(7850.),#4428);
#4456=MEASURE_REPRESENTATION_ITEM('density measure',
POSITIVE_RATIO_MEASURE(7850.),#4429);
#4457=MEASURE_REPRESENTATION_ITEM('density measure',
POSITIVE_RATIO_MEASURE(7850.),#4430);
#4458=MEASURE_REPRESENTATION_ITEM('density measure',
POSITIVE_RATIO_MEASURE(7850.),#4431);
#4459=MEASURE_REPRESENTATION_ITEM('density measure',
POSITIVE_RATIO_MEASURE(7850.),#4432);
#4460=MEASURE_REPRESENTATION_ITEM('density measure',
POSITIVE_RATIO_MEASURE(7850.),#4433);
#4461=MEASURE_REPRESENTATION_ITEM('density measure',
POSITIVE_RATIO_MEASURE(7850.),#4434);
#4462=MEASURE_REPRESENTATION_ITEM('density measure',
POSITIVE_RATIO_MEASURE(7850.),#4435);
#4463=MEASURE_REPRESENTATION_ITEM('density measure',
POSITIVE_RATIO_MEASURE(7850.),#4436);
#4464=PROPERTY_DEFINITION_REPRESENTATION(#4599,#4518);
#4465=PROPERTY_DEFINITION_REPRESENTATION(#4600,#4519);
#4466=PROPERTY_DEFINITION_REPRESENTATION(#4601,#4520);
#4467=PROPERTY_DEFINITION_REPRESENTATION(#4602,#4521);
#4468=PROPERTY_DEFINITION_REPRESENTATION(#4603,#4522);
#4469=PROPERTY_DEFINITION_REPRESENTATION(#4604,#4523);
#4470=PROPERTY_DEFINITION_REPRESENTATION(#4605,#4524);
#4471=PROPERTY_DEFINITION_REPRESENTATION(#4606,#4525);
#4472=PROPERTY_DEFINITION_REPRESENTATION(#4607,#4526);
#4473=PROPERTY_DEFINITION_REPRESENTATION(#4608,#4527);
#4474=PROPERTY_DEFINITION_REPRESENTATION(#4609,#4528);
#4475=PROPERTY_DEFINITION_REPRESENTATION(#4610,#4529);
#4476=PROPERTY_DEFINITION_REPRESENTATION(#4611,#4530);
#4477=PROPERTY_DEFINITION_REPRESENTATION(#4612,#4531);
#4478=PROPERTY_DEFINITION_REPRESENTATION(#4613,#4532);
#4479=PROPERTY_DEFINITION_REPRESENTATION(#4614,#4533);
#4480=PROPERTY_DEFINITION_REPRESENTATION(#4615,#4534);
#4481=PROPERTY_DEFINITION_REPRESENTATION(#4616,#4535);
#4482=PROPERTY_DEFINITION_REPRESENTATION(#4617,#4536);
#4483=PROPERTY_DEFINITION_REPRESENTATION(#4618,#4537);
#4484=PROPERTY_DEFINITION_REPRESENTATION(#4619,#4538);
#4485=PROPERTY_DEFINITION_REPRESENTATION(#4620,#4539);
#4486=PROPERTY_DEFINITION_REPRESENTATION(#4621,#4540);
#4487=PROPERTY_DEFINITION_REPRESENTATION(#4622,#4541);
#4488=PROPERTY_DEFINITION_REPRESENTATION(#4623,#4542);
#4489=PROPERTY_DEFINITION_REPRESENTATION(#4624,#4543);
#4490=PROPERTY_DEFINITION_REPRESENTATION(#4625,#4544);
#4491=PROPERTY_DEFINITION_REPRESENTATION(#4626,#4545);
#4492=PROPERTY_DEFINITION_REPRESENTATION(#4627,#4546);
#4493=PROPERTY_DEFINITION_REPRESENTATION(#4628,#4547);
#4494=PROPERTY_DEFINITION_REPRESENTATION(#4629,#4548);
#4495=PROPERTY_DEFINITION_REPRESENTATION(#4630,#4549);
#4496=PROPERTY_DEFINITION_REPRESENTATION(#4631,#4550);
#4497=PROPERTY_DEFINITION_REPRESENTATION(#4632,#4551);
#4498=PROPERTY_DEFINITION_REPRESENTATION(#4633,#4552);
#4499=PROPERTY_DEFINITION_REPRESENTATION(#4634,#4553);
#4500=PROPERTY_DEFINITION_REPRESENTATION(#4635,#4554);
#4501=PROPERTY_DEFINITION_REPRESENTATION(#4636,#4555);
#4502=PROPERTY_DEFINITION_REPRESENTATION(#4637,#4556);
#4503=PROPERTY_DEFINITION_REPRESENTATION(#4638,#4557);
#4504=PROPERTY_DEFINITION_REPRESENTATION(#4639,#4558);
#4505=PROPERTY_DEFINITION_REPRESENTATION(#4640,#4559);
#4506=PROPERTY_DEFINITION_REPRESENTATION(#4641,#4560);
#4507=PROPERTY_DEFINITION_REPRESENTATION(#4642,#4561);
#4508=PROPERTY_DEFINITION_REPRESENTATION(#4643,#4562);
#4509=PROPERTY_DEFINITION_REPRESENTATION(#4644,#4563);
#4510=PROPERTY_DEFINITION_REPRESENTATION(#4645,#4564);
#4511=PROPERTY_DEFINITION_REPRESENTATION(#4646,#4565);
#4512=PROPERTY_DEFINITION_REPRESENTATION(#4647,#4566);
#4513=PROPERTY_DEFINITION_REPRESENTATION(#4648,#4567);
#4514=PROPERTY_DEFINITION_REPRESENTATION(#4649,#4568);
#4515=PROPERTY_DEFINITION_REPRESENTATION(#4650,#4569);
#4516=PROPERTY_DEFINITION_REPRESENTATION(#4651,#4570);
#4517=PROPERTY_DEFINITION_REPRESENTATION(#4652,#4571);
#4518=REPRESENTATION('material name',(#4572),#8348);
#4519=REPRESENTATION('density',(#4437),#8348);
#4520=REPRESENTATION('material name',(#4573),#8349);
#4521=REPRESENTATION('density',(#4438),#8349);
#4522=REPRESENTATION('material name',(#4574),#8350);
#4523=REPRESENTATION('density',(#4439),#8350);
#4524=REPRESENTATION('material name',(#4575),#8351);
#4525=REPRESENTATION('density',(#4440),#8351);
#4526=REPRESENTATION('material name',(#4576),#8352);
#4527=REPRESENTATION('density',(#4441),#8352);
#4528=REPRESENTATION('material name',(#4577),#8353);
#4529=REPRESENTATION('density',(#4442),#8353);
#4530=REPRESENTATION('material name',(#4578),#8354);
#4531=REPRESENTATION('density',(#4443),#8354);
#4532=REPRESENTATION('material name',(#4579),#8355);
#4533=REPRESENTATION('density',(#4444),#8355);
#4534=REPRESENTATION('material name',(#4580),#8356);
#4535=REPRESENTATION('density',(#4445),#8356);
#4536=REPRESENTATION('material name',(#4581),#8357);
#4537=REPRESENTATION('density',(#4446),#8357);
#4538=REPRESENTATION('material name',(#4582),#8358);
#4539=REPRESENTATION('density',(#4447),#8358);
#4540=REPRESENTATION('material name',(#4583),#8359);
#4541=REPRESENTATION('density',(#4448),#8359);
#4542=REPRESENTATION('material name',(#4584),#8360);
#4543=REPRESENTATION('density',(#4449),#8360);
#4544=REPRESENTATION('material name',(#4585),#8362);
#4545=REPRESENTATION('density',(#4450),#8362);
#4546=REPRESENTATION('material name',(#4586),#8363);
#4547=REPRESENTATION('density',(#4451),#8363);
#4548=REPRESENTATION('material name',(#4587),#8364);
#4549=REPRESENTATION('density',(#4452),#8364);
#4550=REPRESENTATION('material name',(#4588),#8365);
#4551=REPRESENTATION('density',(#4453),#8365);
#4552=REPRESENTATION('material name',(#4589),#8367);
#4553=REPRESENTATION('density',(#4454),#8367);
#4554=REPRESENTATION('material name',(#4590),#8368);
#4555=REPRESENTATION('density',(#4455),#8368);
#4556=REPRESENTATION('material name',(#4591),#8369);
#4557=REPRESENTATION('density',(#4456),#8369);
#4558=REPRESENTATION('material name',(#4592),#8370);
#4559=REPRESENTATION('density',(#4457),#8370);
#4560=REPRESENTATION('material name',(#4593),#8371);
#4561=REPRESENTATION('density',(#4458),#8371);
#4562=REPRESENTATION('material name',(#4594),#8372);
#4563=REPRESENTATION('density',(#4459),#8372);
#4564=REPRESENTATION('material name',(#4595),#8373);
#4565=REPRESENTATION('density',(#4460),#8373);
#4566=REPRESENTATION('material name',(#4596),#8374);
#4567=REPRESENTATION('density',(#4461),#8374);
#4568=REPRESENTATION('material name',(#4597),#8375);
#4569=REPRESENTATION('density',(#4462),#8375);
#4570=REPRESENTATION('material name',(#4598),#8376);
#4571=REPRESENTATION('density',(#4463),#8376);
#4572=DESCRIPTIVE_REPRESENTATION_ITEM('Steel','Steel');
#4573=DESCRIPTIVE_REPRESENTATION_ITEM('Steel','Steel');
#4574=DESCRIPTIVE_REPRESENTATION_ITEM('Steel','Steel');
#4575=DESCRIPTIVE_REPRESENTATION_ITEM('Steel','Steel');
#4576=DESCRIPTIVE_REPRESENTATION_ITEM('Steel','Steel');
#4577=DESCRIPTIVE_REPRESENTATION_ITEM('Steel','Steel');
#4578=DESCRIPTIVE_REPRESENTATION_ITEM('Steel','Steel');
#4579=DESCRIPTIVE_REPRESENTATION_ITEM('Steel','Steel');
#4580=DESCRIPTIVE_REPRESENTATION_ITEM('Steel','Steel');
#4581=DESCRIPTIVE_REPRESENTATION_ITEM('Steel','Steel');
#4582=DESCRIPTIVE_REPRESENTATION_ITEM('Steel','Steel');
#4583=DESCRIPTIVE_REPRESENTATION_ITEM('Steel','Steel');
#4584=DESCRIPTIVE_REPRESENTATION_ITEM('Steel','Steel');
#4585=DESCRIPTIVE_REPRESENTATION_ITEM('Steel','Steel');
#4586=DESCRIPTIVE_REPRESENTATION_ITEM('Steel','Steel');
#4587=DESCRIPTIVE_REPRESENTATION_ITEM('Steel','Steel');
#4588=DESCRIPTIVE_REPRESENTATION_ITEM('Steel','Steel');
#4589=DESCRIPTIVE_REPRESENTATION_ITEM('Steel','Steel');
#4590=DESCRIPTIVE_REPRESENTATION_ITEM('Steel','Steel');
#4591=DESCRIPTIVE_REPRESENTATION_ITEM('Steel','Steel');
#4592=DESCRIPTIVE_REPRESENTATION_ITEM('Steel','Steel');
#4593=DESCRIPTIVE_REPRESENTATION_ITEM('Steel','Steel');
#4594=DESCRIPTIVE_REPRESENTATION_ITEM('Steel','Steel');
#4595=DESCRIPTIVE_REPRESENTATION_ITEM('Steel','Steel');
#4596=DESCRIPTIVE_REPRESENTATION_ITEM('Steel','Steel');
#4597=DESCRIPTIVE_REPRESENTATION_ITEM('Steel','Steel');
#4598=DESCRIPTIVE_REPRESENTATION_ITEM('Steel','Steel');
#4599=PROPERTY_DEFINITION('material property','material name',#8531);
#4600=PROPERTY_DEFINITION('material property','density of part',#8531);
#4601=PROPERTY_DEFINITION('material property','material name',#8532);
#4602=PROPERTY_DEFINITION('material property','density of part',#8532);
#4603=PROPERTY_DEFINITION('material property','material name',#8533);
#4604=PROPERTY_DEFINITION('material property','density of part',#8533);
#4605=PROPERTY_DEFINITION('material property','material name',#8534);
#4606=PROPERTY_DEFINITION('material property','density of part',#8534);
#4607=PROPERTY_DEFINITION('material property','material name',#8535);
#4608=PROPERTY_DEFINITION('material property','density of part',#8535);
#4609=PROPERTY_DEFINITION('material property','material name',#8536);
#4610=PROPERTY_DEFINITION('material property','density of part',#8536);
#4611=PROPERTY_DEFINITION('material property','material name',#8537);
#4612=PROPERTY_DEFINITION('material property','density of part',#8537);
#4613=PROPERTY_DEFINITION('material property','material name',#8538);
#4614=PROPERTY_DEFINITION('material property','density of part',#8538);
#4615=PROPERTY_DEFINITION('material property','material name',#8539);
#4616=PROPERTY_DEFINITION('material property','density of part',#8539);
#4617=PROPERTY_DEFINITION('material property','material name',#8540);
#4618=PROPERTY_DEFINITION('material property','density of part',#8540);
#4619=PROPERTY_DEFINITION('material property','material name',#8541);
#4620=PROPERTY_DEFINITION('material property','density of part',#8541);
#4621=PROPERTY_DEFINITION('material property','material name',#8542);
#4622=PROPERTY_DEFINITION('material property','density of part',#8542);
#4623=PROPERTY_DEFINITION('material property','material name',#8543);
#4624=PROPERTY_DEFINITION('material property','density of part',#8543);
#4625=PROPERTY_DEFINITION('material property','material name',#8545);
#4626=PROPERTY_DEFINITION('material property','density of part',#8545);
#4627=PROPERTY_DEFINITION('material property','material name',#8546);
#4628=PROPERTY_DEFINITION('material property','density of part',#8546);
#4629=PROPERTY_DEFINITION('material property','material name',#8547);
#4630=PROPERTY_DEFINITION('material property','density of part',#8547);
#4631=PROPERTY_DEFINITION('material property','material name',#8548);
#4632=PROPERTY_DEFINITION('material property','density of part',#8548);
#4633=PROPERTY_DEFINITION('material property','material name',#8550);
#4634=PROPERTY_DEFINITION('material property','density of part',#8550);
#4635=PROPERTY_DEFINITION('material property','material name',#8551);
#4636=PROPERTY_DEFINITION('material property','density of part',#8551);
#4637=PROPERTY_DEFINITION('material property','material name',#8552);
#4638=PROPERTY_DEFINITION('material property','density of part',#8552);
#4639=PROPERTY_DEFINITION('material property','material name',#8553);
#4640=PROPERTY_DEFINITION('material property','density of part',#8553);
#4641=PROPERTY_DEFINITION('material property','material name',#8554);
#4642=PROPERTY_DEFINITION('material property','density of part',#8554);
#4643=PROPERTY_DEFINITION('material property','material name',#8555);
#4644=PROPERTY_DEFINITION('material property','density of part',#8555);
#4645=PROPERTY_DEFINITION('material property','material name',#8556);
#4646=PROPERTY_DEFINITION('material property','density of part',#8556);
#4647=PROPERTY_DEFINITION('material property','material name',#8557);
#4648=PROPERTY_DEFINITION('material property','density of part',#8557);
#4649=PROPERTY_DEFINITION('material property','material name',#8558);
#4650=PROPERTY_DEFINITION('material property','density of part',#8558);
#4651=PROPERTY_DEFINITION('material property','material name',#8559);
#4652=PROPERTY_DEFINITION('material property','density of part',#8559);
#4653=AXIS2_PLACEMENT_3D('',#6465,#5148,#5149);
#4654=AXIS2_PLACEMENT_3D('',#6466,#5150,#5151);
#4655=AXIS2_PLACEMENT_3D('',#6467,#5152,#5153);
#4656=AXIS2_PLACEMENT_3D('',#6468,#5154,#5155);
#4657=AXIS2_PLACEMENT_3D('',#6470,#5156,#5157);
#4658=AXIS2_PLACEMENT_3D('',#6473,#5159,#5160);
#4659=AXIS2_PLACEMENT_3D('',#6474,#5161,#5162);
#4660=AXIS2_PLACEMENT_3D('',#6476,#5163,#5164);
#4661=AXIS2_PLACEMENT_3D('',#6479,#5166,#5167);
#4662=AXIS2_PLACEMENT_3D('',#6480,#5168,#5169);
#4663=AXIS2_PLACEMENT_3D('',#6482,#5170,#5171);
#4664=AXIS2_PLACEMENT_3D('',#6485,#5173,#5174);
#4665=AXIS2_PLACEMENT_3D('',#6486,#5175,#5176);
#4666=AXIS2_PLACEMENT_3D('',#6488,#5177,#5178);
#4667=AXIS2_PLACEMENT_3D('',#6491,#5180,#5181);
#4668=AXIS2_PLACEMENT_3D('',#6492,#5182,#5183);
#4669=AXIS2_PLACEMENT_3D('',#6494,#5184,#5185);
#4670=AXIS2_PLACEMENT_3D('',#6497,#5187,#5188);
#4671=AXIS2_PLACEMENT_3D('',#6498,#5189,#5190);
#4672=AXIS2_PLACEMENT_3D('',#6500,#5191,#5192);
#4673=AXIS2_PLACEMENT_3D('',#6503,#5194,#5195);
#4674=AXIS2_PLACEMENT_3D('',#6504,#5196,#5197);
#4675=AXIS2_PLACEMENT_3D('',#6506,#5198,#5199);
#4676=AXIS2_PLACEMENT_3D('',#6509,#5201,#5202);
#4677=AXIS2_PLACEMENT_3D('',#6510,#5203,#5204);
#4678=AXIS2_PLACEMENT_3D('',#6512,#5205,#5206);
#4679=AXIS2_PLACEMENT_3D('',#6515,#5208,#5209);
#4680=AXIS2_PLACEMENT_3D('',#6516,#5210,#5211);
#4681=AXIS2_PLACEMENT_3D('',#6518,#5212,#5213);
#4682=AXIS2_PLACEMENT_3D('',#6521,#5215,#5216);
#4683=AXIS2_PLACEMENT_3D('',#6522,#5217,#5218);
#4684=AXIS2_PLACEMENT_3D('',#6524,#5219,#5220);
#4685=AXIS2_PLACEMENT_3D('',#6527,#5222,#5223);
#4686=AXIS2_PLACEMENT_3D('',#6528,#5224,#5225);
#4687=AXIS2_PLACEMENT_3D('',#6537,#5230,#5231);
#4688=AXIS2_PLACEMENT_3D('',#6543,#5235,#5236);
#4689=AXIS2_PLACEMENT_3D('',#6549,#5240,#5241);
#4690=AXIS2_PLACEMENT_3D('',#6552,#5244,#5245);
#4691=AXIS2_PLACEMENT_3D('',#6553,#5246,#5247);
#4692=AXIS2_PLACEMENT_3D('',#6554,#5248,#5249);
#4693=AXIS2_PLACEMENT_3D('',#6555,#5250,#5251);
#4694=AXIS2_PLACEMENT_3D('',#6557,#5252,#5253);
#4695=AXIS2_PLACEMENT_3D('',#6560,#5255,#5256);
#4696=AXIS2_PLACEMENT_3D('',#6561,#5257,#5258);
#4697=AXIS2_PLACEMENT_3D('',#6562,#5259,#5260);
#4698=AXIS2_PLACEMENT_3D('',#6564,#5261,#5262);
#4699=AXIS2_PLACEMENT_3D('',#6567,#5264,#5265);
#4700=AXIS2_PLACEMENT_3D('',#6568,#5266,#5267);
#4701=AXIS2_PLACEMENT_3D('',#6569,#5268,#5269);
#4702=AXIS2_PLACEMENT_3D('',#6578,#5274,#5275);
#4703=AXIS2_PLACEMENT_3D('',#6584,#5279,#5280);
#4704=AXIS2_PLACEMENT_3D('',#6590,#5284,#5285);
#4705=AXIS2_PLACEMENT_3D('',#6593,#5288,#5289);
#4706=AXIS2_PLACEMENT_3D('',#6594,#5290,#5291);
#4707=AXIS2_PLACEMENT_3D('',#6595,#5292,#5293);
#4708=AXIS2_PLACEMENT_3D('',#6596,#5294,#5295);
#4709=AXIS2_PLACEMENT_3D('',#6605,#5300,#5301);
#4710=AXIS2_PLACEMENT_3D('',#6611,#5305,#5306);
#4711=AXIS2_PLACEMENT_3D('',#6617,#5310,#5311);
#4712=AXIS2_PLACEMENT_3D('',#6620,#5314,#5315);
#4713=AXIS2_PLACEMENT_3D('',#6621,#5316,#5317);
#4714=AXIS2_PLACEMENT_3D('',#6622,#5318,#5319);
#4715=AXIS2_PLACEMENT_3D('',#6623,#5320,#5321);
#4716=AXIS2_PLACEMENT_3D('',#6625,#5322,#5323);
#4717=AXIS2_PLACEMENT_3D('',#6628,#5325,#5326);
#4718=AXIS2_PLACEMENT_3D('',#6629,#5327,#5328);
#4719=AXIS2_PLACEMENT_3D('',#6630,#5329,#5330);
#4720=AXIS2_PLACEMENT_3D('',#6632,#5331,#5332);
#4721=AXIS2_PLACEMENT_3D('',#6635,#5334,#5335);
#4722=AXIS2_PLACEMENT_3D('',#6636,#5336,#5337);
#4723=AXIS2_PLACEMENT_3D('',#6637,#5338,#5339);
#4724=AXIS2_PLACEMENT_3D('',#6646,#5344,#5345);
#4725=AXIS2_PLACEMENT_3D('',#6652,#5349,#5350);
#4726=AXIS2_PLACEMENT_3D('',#6658,#5354,#5355);
#4727=AXIS2_PLACEMENT_3D('',#6661,#5358,#5359);
#4728=AXIS2_PLACEMENT_3D('',#6662,#5360,#5361);
#4729=AXIS2_PLACEMENT_3D('',#6663,#5362,#5363);
#4730=AXIS2_PLACEMENT_3D('',#6664,#5364,#5365);
#4731=AXIS2_PLACEMENT_3D('',#6673,#5370,#5371);
#4732=AXIS2_PLACEMENT_3D('',#6679,#5375,#5376);
#4733=AXIS2_PLACEMENT_3D('',#6685,#5380,#5381);
#4734=AXIS2_PLACEMENT_3D('',#6688,#5384,#5385);
#4735=AXIS2_PLACEMENT_3D('',#6689,#5386,#5387);
#4736=AXIS2_PLACEMENT_3D('',#6690,#5388,#5389);
#4737=AXIS2_PLACEMENT_3D('',#6691,#5390,#5391);
#4738=AXIS2_PLACEMENT_3D('',#6693,#5392,#5393);
#4739=AXIS2_PLACEMENT_3D('',#6696,#5395,#5396);
#4740=AXIS2_PLACEMENT_3D('',#6697,#5397,#5398);
#4741=AXIS2_PLACEMENT_3D('',#6699,#5399,#5400);
#4742=AXIS2_PLACEMENT_3D('',#6702,#5402,#5403);
#4743=AXIS2_PLACEMENT_3D('',#6703,#5404,#5405);
#4744=AXIS2_PLACEMENT_3D('',#6704,#5406,#5407);
#4745=AXIS2_PLACEMENT_3D('',#6705,#5408,#5409);
#4746=AXIS2_PLACEMENT_3D('',#6706,#5410,#5411);
#4747=AXIS2_PLACEMENT_3D('',#6708,#5412,#5413);
#4748=AXIS2_PLACEMENT_3D('',#6711,#5415,#5416);
#4749=AXIS2_PLACEMENT_3D('',#6712,#5417,#5418);
#4750=AXIS2_PLACEMENT_3D('',#6714,#5419,#5420);
#4751=AXIS2_PLACEMENT_3D('',#6717,#5422,#5423);
#4752=AXIS2_PLACEMENT_3D('',#6718,#5424,#5425);
#4753=AXIS2_PLACEMENT_3D('',#6719,#5426,#5427);
#4754=AXIS2_PLACEMENT_3D('',#6720,#5428,#5429);
#4755=AXIS2_PLACEMENT_3D('',#6721,#5430,#5431);
#4756=AXIS2_PLACEMENT_3D('',#6723,#5432,#5433);
#4757=AXIS2_PLACEMENT_3D('',#6726,#5435,#5436);
#4758=AXIS2_PLACEMENT_3D('',#6727,#5437,#5438);
#4759=AXIS2_PLACEMENT_3D('',#6729,#5439,#5440);
#4760=AXIS2_PLACEMENT_3D('',#6732,#5442,#5443);
#4761=AXIS2_PLACEMENT_3D('',#6733,#5444,#5445);
#4762=AXIS2_PLACEMENT_3D('',#6734,#5446,#5447);
#4763=AXIS2_PLACEMENT_3D('',#6735,#5448,#5449);
#4764=AXIS2_PLACEMENT_3D('',#6736,#5450,#5451);
#4765=AXIS2_PLACEMENT_3D('',#6738,#5452,#5453);
#4766=AXIS2_PLACEMENT_3D('',#6741,#5455,#5456);
#4767=AXIS2_PLACEMENT_3D('',#6742,#5457,#5458);
#4768=AXIS2_PLACEMENT_3D('',#6744,#5459,#5460);
#4769=AXIS2_PLACEMENT_3D('',#6747,#5462,#5463);
#4770=AXIS2_PLACEMENT_3D('',#6748,#5464,#5465);
#4771=AXIS2_PLACEMENT_3D('',#6749,#5466,#5467);
#4772=AXIS2_PLACEMENT_3D('',#6750,#5468,#5469);
#4773=AXIS2_PLACEMENT_3D('',#6751,#5470,#5471);
#4774=AXIS2_PLACEMENT_3D('',#6753,#5472,#5473);
#4775=AXIS2_PLACEMENT_3D('',#6756,#5475,#5476);
#4776=AXIS2_PLACEMENT_3D('',#6757,#5477,#5478);
#4777=AXIS2_PLACEMENT_3D('',#6759,#5479,#5480);
#4778=AXIS2_PLACEMENT_3D('',#6762,#5482,#5483);
#4779=AXIS2_PLACEMENT_3D('',#6763,#5484,#5485);
#4780=AXIS2_PLACEMENT_3D('',#6764,#5486,#5487);
#4781=AXIS2_PLACEMENT_3D('',#6765,#5488,#5489);
#4782=AXIS2_PLACEMENT_3D('',#6766,#5490,#5491);
#4783=AXIS2_PLACEMENT_3D('',#6768,#5492,#5493);
#4784=AXIS2_PLACEMENT_3D('',#6771,#5495,#5496);
#4785=AXIS2_PLACEMENT_3D('',#6772,#5497,#5498);
#4786=AXIS2_PLACEMENT_3D('',#6774,#5499,#5500);
#4787=AXIS2_PLACEMENT_3D('',#6777,#5502,#5503);
#4788=AXIS2_PLACEMENT_3D('',#6778,#5504,#5505);
#4789=AXIS2_PLACEMENT_3D('',#6779,#5506,#5507);
#4790=AXIS2_PLACEMENT_3D('',#6780,#5508,#5509);
#4791=AXIS2_PLACEMENT_3D('',#6781,#5510,#5511);
#4792=AXIS2_PLACEMENT_3D('',#6783,#5512,#5513);
#4793=AXIS2_PLACEMENT_3D('',#6786,#5515,#5516);
#4794=AXIS2_PLACEMENT_3D('',#6787,#5517,#5518);
#4795=AXIS2_PLACEMENT_3D('',#6789,#5519,#5520);
#4796=AXIS2_PLACEMENT_3D('',#6792,#5522,#5523);
#4797=AXIS2_PLACEMENT_3D('',#6793,#5524,#5525);
#4798=AXIS2_PLACEMENT_3D('',#6794,#5526,#5527);
#4799=AXIS2_PLACEMENT_3D('',#6795,#5528,#5529);
#4800=AXIS2_PLACEMENT_3D('',#6796,#5530,#5531);
#4801=AXIS2_PLACEMENT_3D('',#6798,#5532,#5533);
#4802=AXIS2_PLACEMENT_3D('',#6799,#5534,#5535);
#4803=AXIS2_PLACEMENT_3D('',#6801,#5536,#5537);
#4804=AXIS2_PLACEMENT_3D('',#6803,#5539,#5540);
#4805=AXIS2_PLACEMENT_3D('',#6805,#5541,#5542);
#4806=AXIS2_PLACEMENT_3D('',#6807,#5544,#5545);
#4807=AXIS2_PLACEMENT_3D('',#6809,#5546,#5547);
#4808=AXIS2_PLACEMENT_3D('',#6811,#5549,#5550);
#4809=AXIS2_PLACEMENT_3D('',#6813,#5551,#5552);
#4810=AXIS2_PLACEMENT_3D('',#6814,#5553,#5554);
#4811=AXIS2_PLACEMENT_3D('',#6816,#5555,#5556);
#4812=AXIS2_PLACEMENT_3D('',#6818,#5558,#5559);
#4813=AXIS2_PLACEMENT_3D('',#6820,#5560,#5561);
#4814=AXIS2_PLACEMENT_3D('',#6822,#5563,#5564);
#4815=AXIS2_PLACEMENT_3D('',#6824,#5565,#5566);
#4816=AXIS2_PLACEMENT_3D('',#6826,#5568,#5569);
#4817=AXIS2_PLACEMENT_3D('',#6827,#5570,#5571);
#4818=AXIS2_PLACEMENT_3D('',#6836,#5576,#5577);
#4819=AXIS2_PLACEMENT_3D('',#6842,#5581,#5582);
#4820=AXIS2_PLACEMENT_3D('',#6848,#5586,#5587);
#4821=AXIS2_PLACEMENT_3D('',#6854,#5591,#5592);
#4822=AXIS2_PLACEMENT_3D('',#6860,#5596,#5597);
#4823=AXIS2_PLACEMENT_3D('',#6863,#5600,#5601);
#4824=AXIS2_PLACEMENT_3D('',#6864,#5602,#5603);
#4825=AXIS2_PLACEMENT_3D('',#6865,#5604,#5605);
#4826=AXIS2_PLACEMENT_3D('',#6866,#5606,#5607);
#4827=AXIS2_PLACEMENT_3D('',#6867,#5608,#5609);
#4828=AXIS2_PLACEMENT_3D('',#6869,#5610,#5611);
#4829=AXIS2_PLACEMENT_3D('',#6872,#5613,#5614);
#4830=AXIS2_PLACEMENT_3D('',#6873,#5615,#5616);
#4831=AXIS2_PLACEMENT_3D('',#6875,#5617,#5618);
#4832=AXIS2_PLACEMENT_3D('',#6878,#5620,#5621);
#4833=AXIS2_PLACEMENT_3D('',#6879,#5622,#5623);
#4834=AXIS2_PLACEMENT_3D('',#6882,#5624,#5625);
#4835=AXIS2_PLACEMENT_3D('',#6883,#5626,#5627);
#4836=AXIS2_PLACEMENT_3D('',#6889,#5630,#5631);
#4837=AXIS2_PLACEMENT_3D('',#6890,#5632,#5633);
#4838=AXIS2_PLACEMENT_3D('',#6895,#5635,#5636);
#4839=AXIS2_PLACEMENT_3D('',#6897,#5638,#5639);
#4840=AXIS2_PLACEMENT_3D('',#6902,#5641,#5642);
#4841=AXIS2_PLACEMENT_3D('',#6904,#5644,#5645);
#4842=AXIS2_PLACEMENT_3D('',#6907,#5648,#5649);
#4843=AXIS2_PLACEMENT_3D('',#6913,#5652,#5653);
#4844=AXIS2_PLACEMENT_3D('',#6914,#5654,#5655);
#4845=AXIS2_PLACEMENT_3D('',#6917,#5658,#5659);
#4846=AXIS2_PLACEMENT_3D('',#6927,#5664,#5665);
#4847=AXIS2_PLACEMENT_3D('',#6929,#5666,#5667);
#4848=AXIS2_PLACEMENT_3D('',#6940,#5674,#5675);
#4849=AXIS2_PLACEMENT_3D('',#6941,#5676,#5677);
#4850=AXIS2_PLACEMENT_3D('',#6942,#5678,#5679);
#4851=AXIS2_PLACEMENT_3D('',#6943,#5680,#5681);
#4852=AXIS2_PLACEMENT_3D('',#6944,#5682,#5683);
#4853=AXIS2_PLACEMENT_3D('',#6945,#5684,#5685);
#4854=AXIS2_PLACEMENT_3D('',#6954,#5690,#5691);
#4855=AXIS2_PLACEMENT_3D('',#6960,#5695,#5696);
#4856=AXIS2_PLACEMENT_3D('',#6966,#5700,#5701);
#4857=AXIS2_PLACEMENT_3D('',#6969,#5704,#5705);
#4858=AXIS2_PLACEMENT_3D('',#6970,#5706,#5707);
#4859=AXIS2_PLACEMENT_3D('',#6972,#5708,#5709);
#4860=AXIS2_PLACEMENT_3D('',#6974,#5711,#5712);
#4861=AXIS2_PLACEMENT_3D('',#6976,#5713,#5714);
#4862=AXIS2_PLACEMENT_3D('',#6978,#5716,#5717);
#4863=AXIS2_PLACEMENT_3D('',#6984,#5721,#5722);
#4864=AXIS2_PLACEMENT_3D('',#6988,#5725,#5726);
#4865=AXIS2_PLACEMENT_3D('',#6992,#5729,#5730);
#4866=AXIS2_PLACEMENT_3D('',#6994,#5732,#5733);
#4867=AXIS2_PLACEMENT_3D('',#6995,#5734,#5735);
#4868=AXIS2_PLACEMENT_3D('',#6996,#5736,#5737);
#4869=AXIS2_PLACEMENT_3D('',#6998,#5738,#5739);
#4870=AXIS2_PLACEMENT_3D('',#7001,#5741,#5742);
#4871=AXIS2_PLACEMENT_3D('',#7002,#5743,#5744);
#4872=AXIS2_PLACEMENT_3D('',#7004,#5745,#5746);
#4873=AXIS2_PLACEMENT_3D('',#7005,#5747,#5748);
#4874=AXIS2_PLACEMENT_3D('',#7008,#5749,#5750);
#4875=AXIS2_PLACEMENT_3D('',#7010,#5751,#5752);
#4876=AXIS2_PLACEMENT_3D('',#7011,#5753,#5754);
#4877=AXIS2_PLACEMENT_3D('',#7012,#5755,#5756);
#4878=AXIS2_PLACEMENT_3D('',#7090,#5758,#5759);
#4879=AXIS2_PLACEMENT_3D('',#7168,#5761,#5762);
#4880=AXIS2_PLACEMENT_3D('',#7170,#5763,#5764);
#4881=AXIS2_PLACEMENT_3D('',#7173,#5766,#5767);
#4882=AXIS2_PLACEMENT_3D('',#7338,#5768,#5769);
#4883=AXIS2_PLACEMENT_3D('',#7375,#5771,#5772);
#4884=AXIS2_PLACEMENT_3D('',#7412,#5774,#5775);
#4885=AXIS2_PLACEMENT_3D('',#7449,#5777,#5778);
#4886=AXIS2_PLACEMENT_3D('',#7486,#5780,#5781);
#4887=AXIS2_PLACEMENT_3D('',#7488,#5782,#5783);
#4888=AXIS2_PLACEMENT_3D('',#7489,#5784,#5785);
#4889=AXIS2_PLACEMENT_3D('',#7491,#5786,#5787);
#4890=AXIS2_PLACEMENT_3D('',#7492,#5788,#5789);
#4891=AXIS2_PLACEMENT_3D('',#7494,#5790,#5791);
#4892=AXIS2_PLACEMENT_3D('',#7496,#5793,#5794);
#4893=AXIS2_PLACEMENT_3D('',#7498,#5795,#5796);
#4894=AXIS2_PLACEMENT_3D('',#7499,#5797,#5798);
#4895=AXIS2_PLACEMENT_3D('',#7501,#5800,#5801);
#4896=AXIS2_PLACEMENT_3D('',#7502,#5802,#5803);
#4897=AXIS2_PLACEMENT_3D('',#7503,#5804,#5805);
#4898=AXIS2_PLACEMENT_3D('',#7504,#5806,#5807);
#4899=AXIS2_PLACEMENT_3D('',#7506,#5808,#5809);
#4900=AXIS2_PLACEMENT_3D('',#7509,#5811,#5812);
#4901=AXIS2_PLACEMENT_3D('',#7510,#5813,#5814);
#4902=AXIS2_PLACEMENT_3D('',#7512,#5815,#5816);
#4903=AXIS2_PLACEMENT_3D('',#7515,#5818,#5819);
#4904=AXIS2_PLACEMENT_3D('',#7516,#5820,#5821);
#4905=AXIS2_PLACEMENT_3D('',#7517,#5822,#5823);
#4906=AXIS2_PLACEMENT_3D('',#7518,#5824,#5825);
#4907=AXIS2_PLACEMENT_3D('',#7519,#5826,#5827);
#4908=AXIS2_PLACEMENT_3D('',#7528,#5832,#5833);
#4909=AXIS2_PLACEMENT_3D('',#7534,#5837,#5838);
#4910=AXIS2_PLACEMENT_3D('',#7540,#5842,#5843);
#4911=AXIS2_PLACEMENT_3D('',#7546,#5847,#5848);
#4912=AXIS2_PLACEMENT_3D('',#7552,#5852,#5853);
#4913=AXIS2_PLACEMENT_3D('',#7555,#5856,#5857);
#4914=AXIS2_PLACEMENT_3D('',#7556,#5858,#5859);
#4915=AXIS2_PLACEMENT_3D('',#7557,#5860,#5861);
#4916=AXIS2_PLACEMENT_3D('',#7559,#5862,#5863);
#4917=AXIS2_PLACEMENT_3D('',#7560,#5864,#5865);
#4918=AXIS2_PLACEMENT_3D('',#7562,#5866,#5867);
#4919=AXIS2_PLACEMENT_3D('',#7563,#5868,#5869);
#4920=AXIS2_PLACEMENT_3D('',#7565,#5870,#5871);
#4921=AXIS2_PLACEMENT_3D('',#7567,#5873,#5874);
#4922=AXIS2_PLACEMENT_3D('',#7569,#5875,#5876);
#4923=AXIS2_PLACEMENT_3D('',#7571,#5878,#5879);
#4924=AXIS2_PLACEMENT_3D('',#7573,#5880,#5881);
#4925=AXIS2_PLACEMENT_3D('',#7575,#5883,#5884);
#4926=AXIS2_PLACEMENT_3D('',#7577,#5885,#5886);
#4927=AXIS2_PLACEMENT_3D('',#7578,#5887,#5888);
#4928=AXIS2_PLACEMENT_3D('',#7580,#5889,#5890);
#4929=AXIS2_PLACEMENT_3D('',#7582,#5892,#5893);
#4930=AXIS2_PLACEMENT_3D('',#7584,#5895,#5896);
#4931=AXIS2_PLACEMENT_3D('',#7585,#5897,#5898);
#4932=AXIS2_PLACEMENT_3D('',#7586,#5899,#5900);
#4933=AXIS2_PLACEMENT_3D('',#7587,#5901,#5902);
#4934=AXIS2_PLACEMENT_3D('',#7588,#5903,#5904);
#4935=AXIS2_PLACEMENT_3D('',#7589,#5905,#5906);
#4936=AXIS2_PLACEMENT_3D('',#7590,#5907,#5908);
#4937=AXIS2_PLACEMENT_3D('',#7591,#5909,#5910);
#4938=AXIS2_PLACEMENT_3D('',#7592,#5911,#5912);
#4939=AXIS2_PLACEMENT_3D('',#7593,#5913,#5914);
#4940=AXIS2_PLACEMENT_3D('',#7594,#5915,#5916);
#4941=AXIS2_PLACEMENT_3D('',#7595,#5917,#5918);
#4942=AXIS2_PLACEMENT_3D('',#7596,#5919,#5920);
#4943=AXIS2_PLACEMENT_3D('',#7597,#5921,#5922);
#4944=AXIS2_PLACEMENT_3D('',#7598,#5923,#5924);
#4945=AXIS2_PLACEMENT_3D('',#7599,#5925,#5926);
#4946=AXIS2_PLACEMENT_3D('',#7600,#5927,#5928);
#4947=AXIS2_PLACEMENT_3D('',#7601,#5929,#5930);
#4948=AXIS2_PLACEMENT_3D('',#7602,#5931,#5932);
#4949=AXIS2_PLACEMENT_3D('',#7603,#5933,#5934);
#4950=AXIS2_PLACEMENT_3D('',#7604,#5935,#5936);
#4951=AXIS2_PLACEMENT_3D('',#7605,#5937,#5938);
#4952=AXIS2_PLACEMENT_3D('',#7606,#5939,#5940);
#4953=AXIS2_PLACEMENT_3D('',#7607,#5941,#5942);
#4954=AXIS2_PLACEMENT_3D('',#7608,#5943,#5944);
#4955=AXIS2_PLACEMENT_3D('',#7609,#5945,#5946);
#4956=AXIS2_PLACEMENT_3D('',#7610,#5947,#5948);
#4957=AXIS2_PLACEMENT_3D('',#7611,#5949,#5950);
#4958=AXIS2_PLACEMENT_3D('',#7612,#5951,#5952);
#4959=AXIS2_PLACEMENT_3D('',#7613,#5953,#5954);
#4960=AXIS2_PLACEMENT_3D('',#7614,#5955,#5956);
#4961=AXIS2_PLACEMENT_3D('',#7615,#5957,#5958);
#4962=AXIS2_PLACEMENT_3D('',#7616,#5959,#5960);
#4963=AXIS2_PLACEMENT_3D('',#7617,#5961,#5962);
#4964=AXIS2_PLACEMENT_3D('',#7618,#5963,#5964);
#4965=AXIS2_PLACEMENT_3D('',#7619,#5965,#5966);
#4966=AXIS2_PLACEMENT_3D('',#7620,#5967,#5968);
#4967=AXIS2_PLACEMENT_3D('',#7622,#5969,#5970);
#4968=AXIS2_PLACEMENT_3D('',#7625,#5972,#5973);
#4969=AXIS2_PLACEMENT_3D('',#7626,#5974,#5975);
#4970=AXIS2_PLACEMENT_3D('',#7627,#5976,#5977);
#4971=AXIS2_PLACEMENT_3D('',#7629,#5978,#5979);
#4972=AXIS2_PLACEMENT_3D('',#7632,#5981,#5982);
#4973=AXIS2_PLACEMENT_3D('',#7633,#5983,#5984);
#4974=AXIS2_PLACEMENT_3D('',#7634,#5985,#5986);
#4975=AXIS2_PLACEMENT_3D('',#7643,#5991,#5992);
#4976=AXIS2_PLACEMENT_3D('',#7645,#5993,#5994);
#4977=AXIS2_PLACEMENT_3D('',#7649,#5997,#5998);
#4978=AXIS2_PLACEMENT_3D('',#7655,#6002,#6003);
#4979=AXIS2_PLACEMENT_3D('',#7657,#6005,#6006);
#4980=AXIS2_PLACEMENT_3D('',#7658,#6007,#6008);
#4981=AXIS2_PLACEMENT_3D('',#7659,#6009,#6010);
#4982=AXIS2_PLACEMENT_3D('',#7668,#6015,#6016);
#4983=AXIS2_PLACEMENT_3D('',#7670,#6017,#6018);
#4984=AXIS2_PLACEMENT_3D('',#7674,#6021,#6022);
#4985=AXIS2_PLACEMENT_3D('',#7680,#6026,#6027);
#4986=AXIS2_PLACEMENT_3D('',#7682,#6029,#6030);
#4987=AXIS2_PLACEMENT_3D('',#7683,#6031,#6032);
#4988=AXIS2_PLACEMENT_3D('',#7684,#6033,#6034);
#4989=AXIS2_PLACEMENT_3D('',#7686,#6035,#6036);
#4990=AXIS2_PLACEMENT_3D('',#7689,#6038,#6039);
#4991=AXIS2_PLACEMENT_3D('',#7690,#6040,#6041);
#4992=AXIS2_PLACEMENT_3D('',#7691,#6042,#6043);
#4993=AXIS2_PLACEMENT_3D('',#7692,#6044,#6045);
#4994=AXIS2_PLACEMENT_3D('',#7693,#6046,#6047);
#4995=AXIS2_PLACEMENT_3D('',#7697,#6049,#6050);
#4996=AXIS2_PLACEMENT_3D('',#7698,#6051,#6052);
#4997=AXIS2_PLACEMENT_3D('',#7711,#6053,#6054);
#4998=AXIS2_PLACEMENT_3D('',#7752,#6056,#6057);
#4999=AXIS2_PLACEMENT_3D('',#7763,#6058,#6059);
#5000=AXIS2_PLACEMENT_3D('',#7765,#6061,#6062);
#5001=AXIS2_PLACEMENT_3D('',#7774,#6067,#6068);
#5002=AXIS2_PLACEMENT_3D('',#7780,#6072,#6073);
#5003=AXIS2_PLACEMENT_3D('',#7786,#6077,#6078);
#5004=AXIS2_PLACEMENT_3D('',#7788,#6079,#6080);
#5005=AXIS2_PLACEMENT_3D('',#7789,#6081,#6082);
#5006=AXIS2_PLACEMENT_3D('',#7790,#6083,#6084);
#5007=AXIS2_PLACEMENT_3D('',#7791,#6085,#6086);
#5008=AXIS2_PLACEMENT_3D('',#7792,#6087,#6088);
#5009=AXIS2_PLACEMENT_3D('',#7795,#6090,#6091);
#5010=AXIS2_PLACEMENT_3D('',#7796,#6092,#6093);
#5011=AXIS2_PLACEMENT_3D('',#7797,#6094,#6095);
#5012=AXIS2_PLACEMENT_3D('',#7798,#6096,#6097);
#5013=AXIS2_PLACEMENT_3D('',#7802,#6099,#6100);
#5014=AXIS2_PLACEMENT_3D('',#7803,#6101,#6102);
#5015=AXIS2_PLACEMENT_3D('',#7816,#6103,#6104);
#5016=AXIS2_PLACEMENT_3D('',#7857,#6106,#6107);
#5017=AXIS2_PLACEMENT_3D('',#7868,#6108,#6109);
#5018=AXIS2_PLACEMENT_3D('',#7870,#6111,#6112);
#5019=AXIS2_PLACEMENT_3D('',#7879,#6117,#6118);
#5020=AXIS2_PLACEMENT_3D('',#7885,#6122,#6123);
#5021=AXIS2_PLACEMENT_3D('',#7891,#6127,#6128);
#5022=AXIS2_PLACEMENT_3D('',#7893,#6129,#6130);
#5023=AXIS2_PLACEMENT_3D('',#7894,#6131,#6132);
#5024=AXIS2_PLACEMENT_3D('',#7895,#6133,#6134);
#5025=AXIS2_PLACEMENT_3D('',#7896,#6135,#6136);
#5026=AXIS2_PLACEMENT_3D('',#7897,#6137,#6138);
#5027=AXIS2_PLACEMENT_3D('',#7900,#6140,#6141);
#5028=AXIS2_PLACEMENT_3D('',#7901,#6142,#6143);
#5029=AXIS2_PLACEMENT_3D('',#7902,#6144,#6145);
#5030=AXIS2_PLACEMENT_3D('',#7903,#6146,#6147);
#5031=AXIS2_PLACEMENT_3D('',#7907,#6149,#6150);
#5032=AXIS2_PLACEMENT_3D('',#7908,#6151,#6152);
#5033=AXIS2_PLACEMENT_3D('',#7925,#6153,#6154);
#5034=AXIS2_PLACEMENT_3D('',#7966,#6156,#6157);
#5035=AXIS2_PLACEMENT_3D('',#7981,#6158,#6159);
#5036=AXIS2_PLACEMENT_3D('',#7983,#6161,#6162);
#5037=AXIS2_PLACEMENT_3D('',#7985,#6163,#6164);
#5038=AXIS2_PLACEMENT_3D('',#7988,#6166,#6167);
#5039=AXIS2_PLACEMENT_3D('',#7989,#6168,#6169);
#5040=AXIS2_PLACEMENT_3D('',#7991,#6170,#6171);
#5041=AXIS2_PLACEMENT_3D('',#7994,#6173,#6174);
#5042=AXIS2_PLACEMENT_3D('',#7995,#6175,#6176);
#5043=AXIS2_PLACEMENT_3D('',#7996,#6177,#6178);
#5044=AXIS2_PLACEMENT_3D('',#7997,#6179,#6180);
#5045=AXIS2_PLACEMENT_3D('',#7998,#6181,#6182);
#5046=AXIS2_PLACEMENT_3D('',#8002,#6184,#6185);
#5047=AXIS2_PLACEMENT_3D('',#8003,#6186,#6187);
#5048=AXIS2_PLACEMENT_3D('',#8020,#6188,#6189);
#5049=AXIS2_PLACEMENT_3D('',#8061,#6191,#6192);
#5050=AXIS2_PLACEMENT_3D('',#8076,#6193,#6194);
#5051=AXIS2_PLACEMENT_3D('',#8078,#6196,#6197);
#5052=AXIS2_PLACEMENT_3D('',#8080,#6198,#6199);
#5053=AXIS2_PLACEMENT_3D('',#8083,#6201,#6202);
#5054=AXIS2_PLACEMENT_3D('',#8084,#6203,#6204);
#5055=AXIS2_PLACEMENT_3D('',#8086,#6205,#6206);
#5056=AXIS2_PLACEMENT_3D('',#8089,#6208,#6209);
#5057=AXIS2_PLACEMENT_3D('',#8090,#6210,#6211);
#5058=AXIS2_PLACEMENT_3D('',#8091,#6212,#6213);
#5059=AXIS2_PLACEMENT_3D('',#8092,#6214,#6215);
#5060=AXIS2_PLACEMENT_3D('',#8093,#6216,#6217);
#5061=AXIS2_PLACEMENT_3D('',#8095,#6218,#6219);
#5062=AXIS2_PLACEMENT_3D('',#8098,#6221,#6222);
#5063=AXIS2_PLACEMENT_3D('',#8099,#6223,#6224);
#5064=AXIS2_PLACEMENT_3D('',#8101,#6225,#6226);
#5065=AXIS2_PLACEMENT_3D('',#8104,#6228,#6229);
#5066=AXIS2_PLACEMENT_3D('',#8105,#6230,#6231);
#5067=AXIS2_PLACEMENT_3D('',#8106,#6232,#6233);
#5068=AXIS2_PLACEMENT_3D('',#8107,#6234,#6235);
#5069=AXIS2_PLACEMENT_3D('',#8108,#6236,#6237);
#5070=AXIS2_PLACEMENT_3D('',#8110,#6238,#6239);
#5071=AXIS2_PLACEMENT_3D('',#8113,#6241,#6242);
#5072=AXIS2_PLACEMENT_3D('',#8114,#6243,#6244);
#5073=AXIS2_PLACEMENT_3D('',#8116,#6245,#6246);
#5074=AXIS2_PLACEMENT_3D('',#8119,#6248,#6249);
#5075=AXIS2_PLACEMENT_3D('',#8120,#6250,#6251);
#5076=AXIS2_PLACEMENT_3D('',#8121,#6252,#6253);
#5077=AXIS2_PLACEMENT_3D('',#8122,#6254,#6255);
#5078=AXIS2_PLACEMENT_3D('',#8123,#6256,#6257);
#5079=AXIS2_PLACEMENT_3D('',#8140,#6266,#6267);
#5080=AXIS2_PLACEMENT_3D('',#8146,#6271,#6272);
#5081=AXIS2_PLACEMENT_3D('',#8150,#6275,#6276);
#5082=AXIS2_PLACEMENT_3D('',#8154,#6279,#6280);
#5083=AXIS2_PLACEMENT_3D('',#8158,#6283,#6284);
#5084=AXIS2_PLACEMENT_3D('',#8166,#6289,#6290);
#5085=AXIS2_PLACEMENT_3D('',#8168,#6292,#6293);
#5086=AXIS2_PLACEMENT_3D('',#8170,#6295,#6296);
#5087=AXIS2_PLACEMENT_3D('',#8172,#6298,#6299);
#5088=AXIS2_PLACEMENT_3D('',#8173,#6300,#6301);
#5089=AXIS2_PLACEMENT_3D('',#8174,#6302,#6303);
#5090=AXIS2_PLACEMENT_3D('',#8183,#6308,#6309);
#5091=AXIS2_PLACEMENT_3D('',#8189,#6313,#6314);
#5092=AXIS2_PLACEMENT_3D('',#8195,#6318,#6319);
#5093=AXIS2_PLACEMENT_3D('',#8201,#6323,#6324);
#5094=AXIS2_PLACEMENT_3D('',#8207,#6328,#6329);
#5095=AXIS2_PLACEMENT_3D('',#8210,#6332,#6333);
#5096=AXIS2_PLACEMENT_3D('',#8211,#6334,#6335);
#5097=AXIS2_PLACEMENT_3D('',#8213,#6336,#6337);
#5098=AXIS2_PLACEMENT_3D('',#8214,#6338,#6339);
#5099=AXIS2_PLACEMENT_3D('',#8216,#6340,#6341);
#5100=AXIS2_PLACEMENT_3D('',#8218,#6343,#6344);
#5101=AXIS2_PLACEMENT_3D('',#8220,#6345,#6346);
#5102=AXIS2_PLACEMENT_3D('',#8222,#6348,#6349);
#5103=AXIS2_PLACEMENT_3D('',#8224,#6350,#6351);
#5104=AXIS2_PLACEMENT_3D('',#8226,#6353,#6354);
#5105=AXIS2_PLACEMENT_3D('',#8227,#6355,#6356);
#5106=AXIS2_PLACEMENT_3D('',#8228,#6357,#6358);
#5107=AXIS2_PLACEMENT_3D('',#8230,#6359,#6360);
#5108=AXIS2_PLACEMENT_3D('',#8231,#6361,#6362);
#5109=AXIS2_PLACEMENT_3D('',#8233,#6363,#6364);
#5110=AXIS2_PLACEMENT_3D('',#8235,#6366,#6367);
#5111=AXIS2_PLACEMENT_3D('',#8237,#6368,#6369);
#5112=AXIS2_PLACEMENT_3D('',#8239,#6371,#6372);
#5113=AXIS2_PLACEMENT_3D('',#8241,#6373,#6374);
#5114=AXIS2_PLACEMENT_3D('',#8243,#6376,#6377);
#5115=AXIS2_PLACEMENT_3D('',#8245,#6378,#6379);
#5116=AXIS2_PLACEMENT_3D('',#8246,#6380,#6381);
#5117=AXIS2_PLACEMENT_3D('',#8248,#6382,#6383);
#5118=AXIS2_PLACEMENT_3D('',#8250,#6385,#6386);
#5119=AXIS2_PLACEMENT_3D('',#8252,#6387,#6388);
#5120=AXIS2_PLACEMENT_3D('',#8254,#6390,#6391);
#5121=AXIS2_PLACEMENT_3D('',#8256,#6392,#6393);
#5122=AXIS2_PLACEMENT_3D('',#8258,#6395,#6396);
#5123=AXIS2_PLACEMENT_3D('',#8259,#6397,#6398);
#5124=AXIS2_PLACEMENT_3D('',#8268,#6403,#6404);
#5125=AXIS2_PLACEMENT_3D('',#8274,#6408,#6409);
#5126=AXIS2_PLACEMENT_3D('',#8280,#6413,#6414);
#5127=AXIS2_PLACEMENT_3D('',#8286,#6418,#6419);
#5128=AXIS2_PLACEMENT_3D('',#8292,#6423,#6424);
#5129=AXIS2_PLACEMENT_3D('',#8295,#6427,#6428);
#5130=AXIS2_PLACEMENT_3D('',#8296,#6429,#6430);
#5131=AXIS2_PLACEMENT_3D('',#8297,#6431,#6432);
#5132=AXIS2_PLACEMENT_3D('',#8298,#6433,#6434);
#5133=AXIS2_PLACEMENT_3D('',#8299,#6435,#6436);
#5134=AXIS2_PLACEMENT_3D('',#8300,#6437,#6438);
#5135=AXIS2_PLACEMENT_3D('',#8301,#6439,#6440);
#5136=AXIS2_PLACEMENT_3D('',#8302,#6441,#6442);
#5137=AXIS2_PLACEMENT_3D('',#8303,#6443,#6444);
#5138=AXIS2_PLACEMENT_3D('',#8304,#6445,#6446);
#5139=AXIS2_PLACEMENT_3D('',#8305,#6447,#6448);
#5140=AXIS2_PLACEMENT_3D('',#8306,#6449,#6450);
#5141=AXIS2_PLACEMENT_3D('',#8307,#6451,#6452);
#5142=AXIS2_PLACEMENT_3D('',#8308,#6453,#6454);
#5143=AXIS2_PLACEMENT_3D('',#8309,#6455,#6456);
#5144=AXIS2_PLACEMENT_3D('',#8310,#6457,#6458);
#5145=AXIS2_PLACEMENT_3D('',#8311,#6459,#6460);
#5146=AXIS2_PLACEMENT_3D('',#8312,#6461,#6462);
#5147=AXIS2_PLACEMENT_3D('',#8313,#6463,#6464);
#5148=DIRECTION('axis',(0.,0.,1.));
#5149=DIRECTION('refdir',(1.,0.,0.));
#5150=DIRECTION('axis',(0.,0.,1.));
#5151=DIRECTION('refdir',(1.,0.,0.));
#5152=DIRECTION('axis',(0.,0.,1.));
#5153=DIRECTION('refdir',(1.,0.,0.));
#5154=DIRECTION('center_axis',(0.,0.,1.));
#5155=DIRECTION('ref_axis',(1.,0.,0.));
#5156=DIRECTION('center_axis',(0.,0.,1.));
#5157=DIRECTION('ref_axis',(1.,0.,0.));
#5158=DIRECTION('',(0.,0.,1.));
#5159=DIRECTION('center_axis',(0.,0.,-1.));
#5160=DIRECTION('ref_axis',(1.,0.,0.));
#5161=DIRECTION('center_axis',(0.,0.,1.));
#5162=DIRECTION('ref_axis',(1.,0.,0.));
#5163=DIRECTION('center_axis',(0.,0.,1.));
#5164=DIRECTION('ref_axis',(1.,0.,0.));
#5165=DIRECTION('',(0.,0.,1.));
#5166=DIRECTION('center_axis',(0.,0.,-1.));
#5167=DIRECTION('ref_axis',(1.,0.,0.));
#5168=DIRECTION('center_axis',(0.,0.,1.));
#5169=DIRECTION('ref_axis',(1.,0.,0.));
#5170=DIRECTION('center_axis',(0.,0.,1.));
#5171=DIRECTION('ref_axis',(1.,0.,0.));
#5172=DIRECTION('',(0.,0.,1.));
#5173=DIRECTION('center_axis',(0.,0.,-1.));
#5174=DIRECTION('ref_axis',(1.,0.,0.));
#5175=DIRECTION('center_axis',(0.,0.,1.));
#5176=DIRECTION('ref_axis',(1.,0.,0.));
#5177=DIRECTION('center_axis',(0.,0.,1.));
#5178=DIRECTION('ref_axis',(1.,0.,0.));
#5179=DIRECTION('',(0.,0.,1.));
#5180=DIRECTION('center_axis',(0.,0.,-1.));
#5181=DIRECTION('ref_axis',(1.,0.,0.));
#5182=DIRECTION('center_axis',(0.,0.,1.));
#5183=DIRECTION('ref_axis',(1.,0.,0.));
#5184=DIRECTION('center_axis',(0.,0.,1.));
#5185=DIRECTION('ref_axis',(1.,0.,0.));
#5186=DIRECTION('',(0.,0.,1.));
#5187=DIRECTION('center_axis',(0.,0.,-1.));
#5188=DIRECTION('ref_axis',(1.,0.,0.));
#5189=DIRECTION('center_axis',(0.,0.,1.));
#5190=DIRECTION('ref_axis',(1.,0.,0.));
#5191=DIRECTION('center_axis',(0.,0.,1.));
#5192=DIRECTION('ref_axis',(1.,0.,0.));
#5193=DIRECTION('',(0.,0.,1.));
#5194=DIRECTION('center_axis',(0.,0.,-1.));
#5195=DIRECTION('ref_axis',(1.,0.,0.));
#5196=DIRECTION('center_axis',(0.,0.,1.));
#5197=DIRECTION('ref_axis',(1.,0.,0.));
#5198=DIRECTION('center_axis',(0.,0.,1.));
#5199=DIRECTION('ref_axis',(1.,0.,0.));
#5200=DIRECTION('',(0.,0.,1.));
#5201=DIRECTION('center_axis',(0.,0.,-1.));
#5202=DIRECTION('ref_axis',(1.,0.,0.));
#5203=DIRECTION('center_axis',(0.,0.,1.));
#5204=DIRECTION('ref_axis',(1.,0.,0.));
#5205=DIRECTION('center_axis',(0.,0.,1.));
#5206=DIRECTION('ref_axis',(1.,0.,0.));
#5207=DIRECTION('',(0.,0.,1.));
#5208=DIRECTION('center_axis',(0.,0.,-1.));
#5209=DIRECTION('ref_axis',(1.,0.,0.));
#5210=DIRECTION('center_axis',(0.,0.,1.));
#5211=DIRECTION('ref_axis',(1.,0.,0.));
#5212=DIRECTION('center_axis',(0.,0.,1.));
#5213=DIRECTION('ref_axis',(1.,0.,0.));
#5214=DIRECTION('',(0.,0.,1.));
#5215=DIRECTION('center_axis',(0.,0.,-1.));
#5216=DIRECTION('ref_axis',(1.,0.,0.));
#5217=DIRECTION('center_axis',(0.,0.,1.));
#5218=DIRECTION('ref_axis',(1.,0.,0.));
#5219=DIRECTION('center_axis',(0.,0.,1.));
#5220=DIRECTION('ref_axis',(1.,0.,0.));
#5221=DIRECTION('',(0.,0.,1.));
#5222=DIRECTION('center_axis',(0.,0.,-1.));
#5223=DIRECTION('ref_axis',(1.,0.,0.));
#5224=DIRECTION('center_axis',(0.,1.,0.));
#5225=DIRECTION('ref_axis',(-1.,0.,0.));
#5226=DIRECTION('',(-1.,0.,0.));
#5227=DIRECTION('',(0.,0.,1.));
#5228=DIRECTION('',(-1.,0.,0.));
#5229=DIRECTION('',(0.,0.,1.));
#5230=DIRECTION('center_axis',(1.,0.,0.));
#5231=DIRECTION('ref_axis',(0.,1.,0.));
#5232=DIRECTION('',(0.,1.,0.));
#5233=DIRECTION('',(0.,1.,0.));
#5234=DIRECTION('',(0.,0.,1.));
#5235=DIRECTION('center_axis',(0.,-1.,0.));
#5236=DIRECTION('ref_axis',(1.,0.,0.));
#5237=DIRECTION('',(1.,0.,0.));
#5238=DIRECTION('',(1.,0.,0.));
#5239=DIRECTION('',(0.,0.,1.));
#5240=DIRECTION('center_axis',(-1.,0.,0.));
#5241=DIRECTION('ref_axis',(0.,-1.,0.));
#5242=DIRECTION('',(0.,-1.,0.));
#5243=DIRECTION('',(0.,-1.,0.));
#5244=DIRECTION('center_axis',(0.,0.,1.));
#5245=DIRECTION('ref_axis',(1.,0.,0.));
#5246=DIRECTION('center_axis',(0.,0.,1.));
#5247=DIRECTION('ref_axis',(1.,0.,0.));
#5248=DIRECTION('axis',(0.,0.,1.));
#5249=DIRECTION('refdir',(1.,0.,0.));
#5250=DIRECTION('center_axis',(0.,0.,1.));
#5251=DIRECTION('ref_axis',(1.,0.,0.));
#5252=DIRECTION('center_axis',(0.,0.,1.));
#5253=DIRECTION('ref_axis',(1.,0.,0.));
#5254=DIRECTION('',(0.,0.,1.));
#5255=DIRECTION('center_axis',(0.,0.,-1.));
#5256=DIRECTION('ref_axis',(1.,0.,0.));
#5257=DIRECTION('center_axis',(0.,0.,1.));
#5258=DIRECTION('ref_axis',(1.,0.,0.));
#5259=DIRECTION('center_axis',(0.,0.,1.));
#5260=DIRECTION('ref_axis',(1.,0.,0.));
#5261=DIRECTION('center_axis',(0.,0.,1.));
#5262=DIRECTION('ref_axis',(1.,0.,0.));
#5263=DIRECTION('',(0.,0.,1.));
#5264=DIRECTION('center_axis',(0.,0.,-1.));
#5265=DIRECTION('ref_axis',(1.,0.,0.));
#5266=DIRECTION('center_axis',(0.,0.,1.));
#5267=DIRECTION('ref_axis',(1.,0.,0.));
#5268=DIRECTION('center_axis',(0.,1.,0.));
#5269=DIRECTION('ref_axis',(-1.,0.,0.));
#5270=DIRECTION('',(-1.,0.,0.));
#5271=DIRECTION('',(0.,0.,1.));
#5272=DIRECTION('',(-1.,0.,0.));
#5273=DIRECTION('',(0.,0.,1.));
#5274=DIRECTION('center_axis',(1.,0.,0.));
#5275=DIRECTION('ref_axis',(0.,1.,0.));
#5276=DIRECTION('',(0.,1.,0.));
#5277=DIRECTION('',(0.,1.,0.));
#5278=DIRECTION('',(0.,0.,1.));
#5279=DIRECTION('center_axis',(0.,-1.,0.));
#5280=DIRECTION('ref_axis',(1.,0.,0.));
#5281=DIRECTION('',(1.,0.,0.));
#5282=DIRECTION('',(1.,0.,0.));
#5283=DIRECTION('',(0.,0.,1.));
#5284=DIRECTION('center_axis',(-1.,0.,0.));
#5285=DIRECTION('ref_axis',(0.,-1.,0.));
#5286=DIRECTION('',(0.,-1.,0.));
#5287=DIRECTION('',(0.,-1.,0.));
#5288=DIRECTION('center_axis',(0.,0.,1.));
#5289=DIRECTION('ref_axis',(1.,0.,0.));
#5290=DIRECTION('center_axis',(0.,0.,1.));
#5291=DIRECTION('ref_axis',(1.,0.,0.));
#5292=DIRECTION('axis',(0.,0.,1.));
#5293=DIRECTION('refdir',(1.,0.,0.));
#5294=DIRECTION('center_axis',(0.,1.,0.));
#5295=DIRECTION('ref_axis',(-1.,0.,0.));
#5296=DIRECTION('',(-1.,0.,0.));
#5297=DIRECTION('',(0.,0.,1.));
#5298=DIRECTION('',(-1.,0.,0.));
#5299=DIRECTION('',(0.,0.,1.));
#5300=DIRECTION('center_axis',(1.,0.,0.));
#5301=DIRECTION('ref_axis',(0.,1.,0.));
#5302=DIRECTION('',(0.,1.,0.));
#5303=DIRECTION('',(0.,1.,0.));
#5304=DIRECTION('',(0.,0.,1.));
#5305=DIRECTION('center_axis',(0.,-1.,0.));
#5306=DIRECTION('ref_axis',(1.,0.,0.));
#5307=DIRECTION('',(1.,0.,0.));
#5308=DIRECTION('',(1.,0.,0.));
#5309=DIRECTION('',(0.,0.,1.));
#5310=DIRECTION('center_axis',(-1.,0.,0.));
#5311=DIRECTION('ref_axis',(0.,-1.,0.));
#5312=DIRECTION('',(0.,-1.,0.));
#5313=DIRECTION('',(0.,-1.,0.));
#5314=DIRECTION('center_axis',(0.,0.,1.));
#5315=DIRECTION('ref_axis',(1.,0.,0.));
#5316=DIRECTION('center_axis',(0.,0.,1.));
#5317=DIRECTION('ref_axis',(1.,0.,0.));
#5318=DIRECTION('axis',(0.,0.,1.));
#5319=DIRECTION('refdir',(1.,0.,0.));
#5320=DIRECTION('center_axis',(0.,0.,1.));
#5321=DIRECTION('ref_axis',(1.,0.,0.));
#5322=DIRECTION('center_axis',(0.,0.,1.));
#5323=DIRECTION('ref_axis',(1.,0.,0.));
#5324=DIRECTION('',(0.,0.,1.));
#5325=DIRECTION('center_axis',(0.,0.,-1.));
#5326=DIRECTION('ref_axis',(1.,0.,0.));
#5327=DIRECTION('center_axis',(0.,0.,1.));
#5328=DIRECTION('ref_axis',(1.,0.,0.));
#5329=DIRECTION('center_axis',(0.,0.,1.));
#5330=DIRECTION('ref_axis',(1.,0.,0.));
#5331=DIRECTION('center_axis',(0.,0.,1.));
#5332=DIRECTION('ref_axis',(1.,0.,0.));
#5333=DIRECTION('',(0.,0.,1.));
#5334=DIRECTION('center_axis',(0.,0.,-1.));
#5335=DIRECTION('ref_axis',(1.,0.,0.));
#5336=DIRECTION('center_axis',(0.,0.,1.));
#5337=DIRECTION('ref_axis',(1.,0.,0.));
#5338=DIRECTION('center_axis',(0.,1.,0.));
#5339=DIRECTION('ref_axis',(-1.,0.,0.));
#5340=DIRECTION('',(-1.,0.,0.));
#5341=DIRECTION('',(0.,0.,1.));
#5342=DIRECTION('',(-1.,0.,0.));
#5343=DIRECTION('',(0.,0.,1.));
#5344=DIRECTION('center_axis',(1.,0.,0.));
#5345=DIRECTION('ref_axis',(0.,1.,0.));
#5346=DIRECTION('',(0.,1.,0.));
#5347=DIRECTION('',(0.,1.,0.));
#5348=DIRECTION('',(0.,0.,1.));
#5349=DIRECTION('center_axis',(0.,-1.,0.));
#5350=DIRECTION('ref_axis',(1.,0.,0.));
#5351=DIRECTION('',(1.,0.,0.));
#5352=DIRECTION('',(1.,0.,0.));
#5353=DIRECTION('',(0.,0.,1.));
#5354=DIRECTION('center_axis',(-1.,0.,0.));
#5355=DIRECTION('ref_axis',(0.,-1.,0.));
#5356=DIRECTION('',(0.,-1.,0.));
#5357=DIRECTION('',(0.,-1.,0.));
#5358=DIRECTION('center_axis',(0.,0.,1.));
#5359=DIRECTION('ref_axis',(1.,0.,0.));
#5360=DIRECTION('center_axis',(0.,0.,1.));
#5361=DIRECTION('ref_axis',(1.,0.,0.));
#5362=DIRECTION('axis',(0.,0.,1.));
#5363=DIRECTION('refdir',(1.,0.,0.));
#5364=DIRECTION('center_axis',(0.,1.,0.));
#5365=DIRECTION('ref_axis',(-1.,0.,0.));
#5366=DIRECTION('',(-1.,0.,0.));
#5367=DIRECTION('',(0.,0.,1.));
#5368=DIRECTION('',(-1.,0.,0.));
#5369=DIRECTION('',(0.,0.,1.));
#5370=DIRECTION('center_axis',(1.,0.,0.));
#5371=DIRECTION('ref_axis',(0.,1.,0.));
#5372=DIRECTION('',(0.,1.,0.));
#5373=DIRECTION('',(0.,1.,0.));
#5374=DIRECTION('',(0.,0.,1.));
#5375=DIRECTION('center_axis',(0.,-1.,0.));
#5376=DIRECTION('ref_axis',(1.,0.,0.));
#5377=DIRECTION('',(1.,0.,0.));
#5378=DIRECTION('',(1.,0.,0.));
#5379=DIRECTION('',(0.,0.,1.));
#5380=DIRECTION('center_axis',(-1.,0.,0.));
#5381=DIRECTION('ref_axis',(0.,-1.,0.));
#5382=DIRECTION('',(0.,-1.,0.));
#5383=DIRECTION('',(0.,-1.,0.));
#5384=DIRECTION('center_axis',(0.,0.,1.));
#5385=DIRECTION('ref_axis',(1.,0.,0.));
#5386=DIRECTION('center_axis',(0.,0.,1.));
#5387=DIRECTION('ref_axis',(1.,0.,0.));
#5388=DIRECTION('axis',(0.,0.,1.));
#5389=DIRECTION('refdir',(1.,0.,0.));
#5390=DIRECTION('center_axis',(0.,0.,1.));
#5391=DIRECTION('ref_axis',(1.,0.,0.));
#5392=DIRECTION('center_axis',(0.,0.,-1.));
#5393=DIRECTION('ref_axis',(1.,0.,0.));
#5394=DIRECTION('',(0.,0.,-1.));
#5395=DIRECTION('center_axis',(0.,0.,-1.));
#5396=DIRECTION('ref_axis',(1.,0.,0.));
#5397=DIRECTION('center_axis',(0.,0.,1.));
#5398=DIRECTION('ref_axis',(1.,0.,0.));
#5399=DIRECTION('center_axis',(0.,0.,1.));
#5400=DIRECTION('ref_axis',(1.,0.,0.));
#5401=DIRECTION('',(0.,0.,-1.));
#5402=DIRECTION('center_axis',(0.,0.,1.));
#5403=DIRECTION('ref_axis',(1.,0.,0.));
#5404=DIRECTION('center_axis',(0.,0.,1.));
#5405=DIRECTION('ref_axis',(1.,0.,0.));
#5406=DIRECTION('center_axis',(0.,0.,1.));
#5407=DIRECTION('ref_axis',(1.,0.,0.));
#5408=DIRECTION('axis',(0.,0.,1.));
#5409=DIRECTION('refdir',(1.,0.,0.));
#5410=DIRECTION('center_axis',(0.,0.,1.));
#5411=DIRECTION('ref_axis',(1.,0.,0.));
#5412=DIRECTION('center_axis',(0.,0.,-1.));
#5413=DIRECTION('ref_axis',(1.,0.,0.));
#5414=DIRECTION('',(0.,0.,-1.));
#5415=DIRECTION('center_axis',(0.,0.,-1.));
#5416=DIRECTION('ref_axis',(1.,0.,0.));
#5417=DIRECTION('center_axis',(0.,0.,1.));
#5418=DIRECTION('ref_axis',(1.,0.,0.));
#5419=DIRECTION('center_axis',(0.,0.,1.));
#5420=DIRECTION('ref_axis',(1.,0.,0.));
#5421=DIRECTION('',(0.,0.,-1.));
#5422=DIRECTION('center_axis',(0.,0.,1.));
#5423=DIRECTION('ref_axis',(1.,0.,0.));
#5424=DIRECTION('center_axis',(0.,0.,1.));
#5425=DIRECTION('ref_axis',(1.,0.,0.));
#5426=DIRECTION('center_axis',(0.,0.,1.));
#5427=DIRECTION('ref_axis',(1.,0.,0.));
#5428=DIRECTION('axis',(0.,0.,1.));
#5429=DIRECTION('refdir',(1.,0.,0.));
#5430=DIRECTION('center_axis',(0.,0.,1.));
#5431=DIRECTION('ref_axis',(1.,0.,0.));
#5432=DIRECTION('center_axis',(0.,0.,-1.));
#5433=DIRECTION('ref_axis',(1.,0.,0.));
#5434=DIRECTION('',(0.,0.,-1.));
#5435=DIRECTION('center_axis',(0.,0.,-1.));
#5436=DIRECTION('ref_axis',(1.,0.,0.));
#5437=DIRECTION('center_axis',(0.,0.,1.));
#5438=DIRECTION('ref_axis',(1.,0.,0.));
#5439=DIRECTION('center_axis',(0.,0.,1.));
#5440=DIRECTION('ref_axis',(1.,0.,0.));
#5441=DIRECTION('',(0.,0.,-1.));
#5442=DIRECTION('center_axis',(0.,0.,1.));
#5443=DIRECTION('ref_axis',(1.,0.,0.));
#5444=DIRECTION('center_axis',(0.,0.,1.));
#5445=DIRECTION('ref_axis',(1.,0.,0.));
#5446=DIRECTION('center_axis',(0.,0.,1.));
#5447=DIRECTION('ref_axis',(1.,0.,0.));
#5448=DIRECTION('axis',(0.,0.,1.));
#5449=DIRECTION('refdir',(1.,0.,0.));
#5450=DIRECTION('center_axis',(0.,0.,1.));
#5451=DIRECTION('ref_axis',(1.,0.,0.));
#5452=DIRECTION('center_axis',(0.,0.,-1.));
#5453=DIRECTION('ref_axis',(1.,0.,0.));
#5454=DIRECTION('',(0.,0.,-1.));
#5455=DIRECTION('center_axis',(0.,0.,-1.));
#5456=DIRECTION('ref_axis',(1.,0.,0.));
#5457=DIRECTION('center_axis',(0.,0.,1.));
#5458=DIRECTION('ref_axis',(1.,0.,0.));
#5459=DIRECTION('center_axis',(0.,0.,1.));
#5460=DIRECTION('ref_axis',(1.,0.,0.));
#5461=DIRECTION('',(0.,0.,-1.));
#5462=DIRECTION('center_axis',(0.,0.,1.));
#5463=DIRECTION('ref_axis',(1.,0.,0.));
#5464=DIRECTION('center_axis',(0.,0.,1.));
#5465=DIRECTION('ref_axis',(1.,0.,0.));
#5466=DIRECTION('center_axis',(0.,0.,1.));
#5467=DIRECTION('ref_axis',(1.,0.,0.));
#5468=DIRECTION('axis',(0.,0.,1.));
#5469=DIRECTION('refdir',(1.,0.,0.));
#5470=DIRECTION('center_axis',(0.,0.,1.));
#5471=DIRECTION('ref_axis',(1.,0.,0.));
#5472=DIRECTION('center_axis',(0.,0.,-1.));
#5473=DIRECTION('ref_axis',(1.,0.,0.));
#5474=DIRECTION('',(0.,0.,-1.));
#5475=DIRECTION('center_axis',(0.,0.,-1.));
#5476=DIRECTION('ref_axis',(1.,0.,0.));
#5477=DIRECTION('center_axis',(0.,0.,1.));
#5478=DIRECTION('ref_axis',(1.,0.,0.));
#5479=DIRECTION('center_axis',(0.,0.,1.));
#5480=DIRECTION('ref_axis',(1.,0.,0.));
#5481=DIRECTION('',(0.,0.,-1.));
#5482=DIRECTION('center_axis',(0.,0.,1.));
#5483=DIRECTION('ref_axis',(1.,0.,0.));
#5484=DIRECTION('center_axis',(0.,0.,1.));
#5485=DIRECTION('ref_axis',(1.,0.,0.));
#5486=DIRECTION('center_axis',(0.,0.,1.));
#5487=DIRECTION('ref_axis',(1.,0.,0.));
#5488=DIRECTION('axis',(0.,0.,1.));
#5489=DIRECTION('refdir',(1.,0.,0.));
#5490=DIRECTION('center_axis',(0.,0.,1.));
#5491=DIRECTION('ref_axis',(1.,0.,0.));
#5492=DIRECTION('center_axis',(0.,0.,-1.));
#5493=DIRECTION('ref_axis',(1.,0.,0.));
#5494=DIRECTION('',(0.,0.,-1.));
#5495=DIRECTION('center_axis',(0.,0.,-1.));
#5496=DIRECTION('ref_axis',(1.,0.,0.));
#5497=DIRECTION('center_axis',(0.,0.,1.));
#5498=DIRECTION('ref_axis',(1.,0.,0.));
#5499=DIRECTION('center_axis',(0.,0.,1.));
#5500=DIRECTION('ref_axis',(1.,0.,0.));
#5501=DIRECTION('',(0.,0.,-1.));
#5502=DIRECTION('center_axis',(0.,0.,1.));
#5503=DIRECTION('ref_axis',(1.,0.,0.));
#5504=DIRECTION('center_axis',(0.,0.,1.));
#5505=DIRECTION('ref_axis',(1.,0.,0.));
#5506=DIRECTION('center_axis',(0.,0.,1.));
#5507=DIRECTION('ref_axis',(1.,0.,0.));
#5508=DIRECTION('axis',(0.,0.,1.));
#5509=DIRECTION('refdir',(1.,0.,0.));
#5510=DIRECTION('center_axis',(0.,1.,0.));
#5511=DIRECTION('ref_axis',(1.,0.,0.));
#5512=DIRECTION('center_axis',(0.,-1.,0.));
#5513=DIRECTION('ref_axis',(1.,0.,0.));
#5514=DIRECTION('',(0.,-1.,0.));
#5515=DIRECTION('center_axis',(0.,-1.,0.));
#5516=DIRECTION('ref_axis',(1.,0.,0.));
#5517=DIRECTION('center_axis',(0.,1.,0.));
#5518=DIRECTION('ref_axis',(1.,0.,0.));
#5519=DIRECTION('center_axis',(0.,1.,0.));
#5520=DIRECTION('ref_axis',(1.,0.,0.));
#5521=DIRECTION('',(0.,-1.,0.));
#5522=DIRECTION('center_axis',(0.,1.,0.));
#5523=DIRECTION('ref_axis',(1.,0.,0.));
#5524=DIRECTION('center_axis',(0.,1.,0.));
#5525=DIRECTION('ref_axis',(1.,0.,0.));
#5526=DIRECTION('center_axis',(0.,1.,0.));
#5527=DIRECTION('ref_axis',(1.,0.,0.));
#5528=DIRECTION('axis',(0.,0.,1.));
#5529=DIRECTION('refdir',(1.,0.,0.));
#5530=DIRECTION('center_axis',(0.,1.,0.));
#5531=DIRECTION('ref_axis',(0.,0.,1.));
#5532=DIRECTION('center_axis',(0.,-1.,0.));
#5533=DIRECTION('ref_axis',(1.,0.,0.));
#5534=DIRECTION('center_axis',(0.,-1.,0.));
#5535=DIRECTION('ref_axis',(1.,0.,0.));
#5536=DIRECTION('center_axis',(0.,-1.,0.));
#5537=DIRECTION('ref_axis',(1.,0.,0.));
#5538=DIRECTION('',(0.707106781186548,0.707106781186547,8.65956056235494E-17));
#5539=DIRECTION('center_axis',(0.,-1.,0.));
#5540=DIRECTION('ref_axis',(1.,0.,0.));
#5541=DIRECTION('center_axis',(0.,-1.,0.));
#5542=DIRECTION('ref_axis',(1.,0.,0.));
#5543=DIRECTION('',(0.,1.,0.));
#5544=DIRECTION('center_axis',(0.,1.,0.));
#5545=DIRECTION('ref_axis',(1.,0.,0.));
#5546=DIRECTION('center_axis',(0.,-1.,0.));
#5547=DIRECTION('ref_axis',(1.,0.,0.));
#5548=DIRECTION('',(-0.707106781186547,0.707106781186548,-8.65956056235493E-17));
#5549=DIRECTION('center_axis',(0.,-1.,0.));
#5550=DIRECTION('ref_axis',(0.,0.,-1.));
#5551=DIRECTION('center_axis',(0.,-1.,0.));
#5552=DIRECTION('ref_axis',(1.,0.,0.));
#5553=DIRECTION('center_axis',(0.,1.,0.));
#5554=DIRECTION('ref_axis',(1.,0.,0.));
#5555=DIRECTION('center_axis',(0.,1.,0.));
#5556=DIRECTION('ref_axis',(1.,0.,0.));
#5557=DIRECTION('',(-0.447213595499958,0.894427190999916,-5.47678698264203E-17));
#5558=DIRECTION('center_axis',(0.,-1.,0.));
#5559=DIRECTION('ref_axis',(1.,0.,0.));
#5560=DIRECTION('center_axis',(0.,1.,0.));
#5561=DIRECTION('ref_axis',(1.,0.,0.));
#5562=DIRECTION('',(0.,1.,0.));
#5563=DIRECTION('center_axis',(0.,1.,0.));
#5564=DIRECTION('ref_axis',(1.,0.,0.));
#5565=DIRECTION('center_axis',(0.,-1.,0.));
#5566=DIRECTION('ref_axis',(1.,0.,0.));
#5567=DIRECTION('',(-0.707106781186547,0.707106781186548,-8.65956056235493E-17));
#5568=DIRECTION('center_axis',(0.,-1.,0.));
#5569=DIRECTION('ref_axis',(0.,0.,-1.));
#5570=DIRECTION('center_axis',(0.866025403784439,0.,-0.5));
#5571=DIRECTION('ref_axis',(0.5,0.,0.866025403784439));
#5572=DIRECTION('',(-0.5,0.,-0.866025403784439));
#5573=DIRECTION('',(0.,-1.,0.));
#5574=DIRECTION('',(0.5,0.,0.866025403784439));
#5575=DIRECTION('',(0.,-1.,0.));
#5576=DIRECTION('center_axis',(1.92296268638356E-16,0.,-1.));
#5577=DIRECTION('ref_axis',(1.,0.,1.92296268638356E-16));
#5578=DIRECTION('',(-1.,0.,-1.92296268638356E-16));
#5579=DIRECTION('',(0.,-1.,0.));
#5580=DIRECTION('',(1.,0.,1.92296268638356E-16));
#5581=DIRECTION('center_axis',(-0.866025403784439,0.,-0.5));
#5582=DIRECTION('ref_axis',(0.5,0.,-0.866025403784439));
#5583=DIRECTION('',(-0.5,0.,0.866025403784438));
#5584=DIRECTION('',(0.,-1.,0.));
#5585=DIRECTION('',(0.5,0.,-0.866025403784438));
#5586=DIRECTION('center_axis',(-0.866025403784439,0.,0.5));
#5587=DIRECTION('ref_axis',(-0.5,0.,-0.866025403784439));
#5588=DIRECTION('',(0.5,0.,0.866025403784439));
#5589=DIRECTION('',(0.,-1.,0.));
#5590=DIRECTION('',(-0.5,0.,-0.866025403784439));
#5591=DIRECTION('center_axis',(-1.92296268638356E-16,0.,1.));
#5592=DIRECTION('ref_axis',(-1.,0.,-1.92296268638356E-16));
#5593=DIRECTION('',(1.,0.,1.92296268638356E-16));
#5594=DIRECTION('',(0.,-1.,0.));
#5595=DIRECTION('',(-1.,0.,-1.92296268638356E-16));
#5596=DIRECTION('center_axis',(0.866025403784439,0.,0.5));
#5597=DIRECTION('ref_axis',(-0.5,0.,0.866025403784439));
#5598=DIRECTION('',(0.5,0.,-0.866025403784439));
#5599=DIRECTION('',(-0.5,0.,0.866025403784439));
#5600=DIRECTION('center_axis',(0.,1.,0.));
#5601=DIRECTION('ref_axis',(1.,0.,0.));
#5602=DIRECTION('center_axis',(0.,-1.,0.));
#5603=DIRECTION('ref_axis',(0.,0.,-1.));
#5604=DIRECTION('axis',(0.,0.,1.));
#5605=DIRECTION('refdir',(1.,0.,0.));
#5606=DIRECTION('axis',(0.,0.,1.));
#5607=DIRECTION('refdir',(1.,0.,0.));
#5608=DIRECTION('center_axis',(0.,1.,0.));
#5609=DIRECTION('ref_axis',(1.,0.,0.));
#5610=DIRECTION('center_axis',(0.,1.,0.));
#5611=DIRECTION('ref_axis',(1.,0.,0.));
#5612=DIRECTION('',(0.,1.,0.));
#5613=DIRECTION('center_axis',(0.,-1.,0.));
#5614=DIRECTION('ref_axis',(1.,0.,0.));
#5615=DIRECTION('center_axis',(0.,1.,0.));
#5616=DIRECTION('ref_axis',(1.,0.,0.));
#5617=DIRECTION('center_axis',(0.,1.,0.));
#5618=DIRECTION('ref_axis',(1.,0.,0.));
#5619=DIRECTION('',(0.,1.,0.));
#5620=DIRECTION('center_axis',(0.,-1.,0.));
#5621=DIRECTION('ref_axis',(1.,0.,0.));
#5622=DIRECTION('center_axis',(6.12323399573677E-17,0.,1.));
#5623=DIRECTION('ref_axis',(1.,0.,0.));
#5624=DIRECTION('center_axis',(-1.22464679914735E-16,1.,0.));
#5625=DIRECTION('ref_axis',(-1.,-1.22464679914735E-16,0.));
#5626=DIRECTION('center_axis',(0.,1.,0.));
#5627=DIRECTION('ref_axis',(0.,0.,1.));
#5628=DIRECTION('',(1.,0.,0.));
#5629=DIRECTION('',(0.850265146687862,0.,0.526354614616295));
#5630=DIRECTION('center_axis',(0.,1.,0.));
#5631=DIRECTION('ref_axis',(1.,0.,0.));
#5632=DIRECTION('center_axis',(0.,1.,0.));
#5633=DIRECTION('ref_axis',(0.,0.,1.));
#5634=DIRECTION('',(1.,0.,0.));
#5635=DIRECTION('center_axis',(0.,1.,0.));
#5636=DIRECTION('ref_axis',(1.,0.,0.));
#5637=DIRECTION('',(0.850265146687862,0.,-0.526354614616295));
#5638=DIRECTION('center_axis',(0.,-1.,0.));
#5639=DIRECTION('ref_axis',(0.,0.,-1.));
#5640=DIRECTION('',(-1.,0.,0.));
#5641=DIRECTION('center_axis',(0.,-1.,0.));
#5642=DIRECTION('ref_axis',(1.,0.,0.));
#5643=DIRECTION('',(-0.850265146687862,0.,-0.526354614616295));
#5644=DIRECTION('center_axis',(-0.526354614616295,0.,0.850265146687862));
#5645=DIRECTION('ref_axis',(0.850265146687862,0.,0.526354614616295));
#5646=DIRECTION('',(0.,1.,0.));
#5647=DIRECTION('',(0.,-1.,0.));
#5648=DIRECTION('center_axis',(0.,-1.,0.));
#5649=DIRECTION('ref_axis',(0.,0.,-1.));
#5650=DIRECTION('',(-1.,0.,0.));
#5651=DIRECTION('',(-0.850265146687862,0.,0.526354614616295));
#5652=DIRECTION('center_axis',(0.,-1.,0.));
#5653=DIRECTION('ref_axis',(1.,0.,0.));
#5654=DIRECTION('center_axis',(0.526354614616295,0.,0.850265146687862));
#5655=DIRECTION('ref_axis',(0.850265146687862,0.,-0.526354614616295));
#5656=DIRECTION('',(0.,-1.,0.));
#5657=DIRECTION('',(0.,1.,0.));
#5658=DIRECTION('center_axis',(0.,0.,1.));
#5659=DIRECTION('ref_axis',(1.,0.,0.));
#5660=DIRECTION('',(0.,-1.,0.));
#5661=DIRECTION('',(1.,0.,0.));
#5662=DIRECTION('',(0.,1.,0.));
#5663=DIRECTION('',(-1.,0.,0.));
#5664=DIRECTION('center_axis',(0.,0.,-1.));
#5665=DIRECTION('ref_axis',(1.,0.,0.));
#5666=DIRECTION('center_axis',(0.,0.,-1.));
#5667=DIRECTION('ref_axis',(1.,0.,0.));
#5668=DIRECTION('',(0.,-1.,0.));
#5669=DIRECTION('',(-1.,0.,0.));
#5670=DIRECTION('',(0.,1.,0.));
#5671=DIRECTION('',(0.,1.,0.));
#5672=DIRECTION('',(1.,0.,0.));
#5673=DIRECTION('',(0.,-1.,0.));
#5674=DIRECTION('center_axis',(0.,1.,0.));
#5675=DIRECTION('ref_axis',(6.12323399573677E-17,0.,1.));
#5676=DIRECTION('center_axis',(0.,1.,0.));
#5677=DIRECTION('ref_axis',(1.,0.,0.));
#5678=DIRECTION('center_axis',(0.,-1.,0.));
#5679=DIRECTION('ref_axis',(1.,0.,0.));
#5680=DIRECTION('center_axis',(0.,1.,0.));
#5681=DIRECTION('ref_axis',(1.,0.,0.));
#5682=DIRECTION('center_axis',(0.,1.,0.));
#5683=DIRECTION('ref_axis',(1.,0.,0.));
#5684=DIRECTION('center_axis',(0.,1.,0.));
#5685=DIRECTION('ref_axis',(-1.,0.,0.));
#5686=DIRECTION('',(-1.,0.,0.));
#5687=DIRECTION('',(0.,0.,1.));
#5688=DIRECTION('',(-1.,0.,0.));
#5689=DIRECTION('',(0.,0.,1.));
#5690=DIRECTION('center_axis',(1.,0.,0.));
#5691=DIRECTION('ref_axis',(0.,1.,0.));
#5692=DIRECTION('',(0.,1.,0.));
#5693=DIRECTION('',(0.,0.,1.));
#5694=DIRECTION('',(0.,1.,0.));
#5695=DIRECTION('center_axis',(0.,-1.,0.));
#5696=DIRECTION('ref_axis',(1.,0.,0.));
#5697=DIRECTION('',(1.,0.,0.));
#5698=DIRECTION('',(0.,0.,1.));
#5699=DIRECTION('',(1.,0.,0.));
#5700=DIRECTION('center_axis',(-1.,0.,0.));
#5701=DIRECTION('ref_axis',(0.,-1.,0.));
#5702=DIRECTION('',(0.,-1.,0.));
#5703=DIRECTION('',(0.,-1.,0.));
#5704=DIRECTION('center_axis',(0.,0.,1.));
#5705=DIRECTION('ref_axis',(1.,0.,0.));
#5706=DIRECTION('center_axis',(0.,0.,1.));
#5707=DIRECTION('ref_axis',(1.,0.,0.));
#5708=DIRECTION('center_axis',(0.,0.,1.));
#5709=DIRECTION('ref_axis',(1.,0.,0.));
#5710=DIRECTION('',(0.,0.,1.));
#5711=DIRECTION('center_axis',(0.,0.,1.));
#5712=DIRECTION('ref_axis',(1.,0.,0.));
#5713=DIRECTION('center_axis',(0.,0.,1.));
#5714=DIRECTION('ref_axis',(1.,0.,0.));
#5715=DIRECTION('',(0.,0.,1.));
#5716=DIRECTION('center_axis',(0.,1.,0.));
#5717=DIRECTION('ref_axis',(-1.,0.,0.));
#5718=DIRECTION('',(-1.,0.,0.));
#5719=DIRECTION('',(0.,0.,1.));
#5720=DIRECTION('',(0.,0.,1.));
#5721=DIRECTION('center_axis',(1.,0.,0.));
#5722=DIRECTION('ref_axis',(0.,1.,0.));
#5723=DIRECTION('',(0.,1.,0.));
#5724=DIRECTION('',(0.,0.,1.));
#5725=DIRECTION('center_axis',(0.,-1.,0.));
#5726=DIRECTION('ref_axis',(1.,0.,0.));
#5727=DIRECTION('',(1.,0.,0.));
#5728=DIRECTION('',(0.,0.,1.));
#5729=DIRECTION('center_axis',(-1.,0.,0.));
#5730=DIRECTION('ref_axis',(0.,-1.,0.));
#5731=DIRECTION('',(0.,-1.,0.));
#5732=DIRECTION('center_axis',(0.,0.,1.));
#5733=DIRECTION('ref_axis',(1.,0.,0.));
#5734=DIRECTION('axis',(0.,0.,1.));
#5735=DIRECTION('refdir',(1.,0.,0.));
#5736=DIRECTION('center_axis',(0.,-1.,0.));
#5737=DIRECTION('ref_axis',(1.,0.,0.));
#5738=DIRECTION('center_axis',(0.,-1.,0.));
#5739=DIRECTION('ref_axis',(1.,0.,0.));
#5740=DIRECTION('',(0.,1.,0.));
#5741=DIRECTION('center_axis',(0.,-1.,0.));
#5742=DIRECTION('ref_axis',(1.,0.,0.));
#5743=DIRECTION('center_axis',(0.,1.,0.));
#5744=DIRECTION('ref_axis',(0.,0.,1.));
#5745=DIRECTION('center_axis',(0.,-1.,0.));
#5746=DIRECTION('ref_axis',(1.,0.,0.));
#5747=DIRECTION('center_axis',(6.12323399573677E-17,0.,1.));
#5748=DIRECTION('ref_axis',(1.,0.,0.));
#5749=DIRECTION('center_axis',(1.22464679914735E-16,-1.,0.));
#5750=DIRECTION('ref_axis',(-1.,-1.22464679914735E-16,0.));
#5751=DIRECTION('center_axis',(0.,-1.,0.));
#5752=DIRECTION('ref_axis',(1.,0.,0.));
#5753=DIRECTION('center_axis',(0.,-1.,0.));
#5754=DIRECTION('ref_axis',(0.,0.,-1.));
#5755=DIRECTION('center_axis',(-0.866025403784438,0.,-0.5));
#5756=DIRECTION('ref_axis',(-0.5,0.,0.866025403784438));
#5757=DIRECTION('',(-0.866025403784438,0.,-0.5));
#5758=DIRECTION('center_axis',(-0.866025403784438,0.,-0.5));
#5759=DIRECTION('ref_axis',(-0.5,0.,0.866025403784438));
#5760=DIRECTION('',(-0.866025403784438,0.,-0.5));
#5761=DIRECTION('center_axis',(0.,-1.,0.));
#5762=DIRECTION('ref_axis',(1.,0.,0.));
#5763=DIRECTION('center_axis',(0.,-1.,0.));
#5764=DIRECTION('ref_axis',(1.,0.,0.));
#5765=DIRECTION('',(0.,1.,0.));
#5766=DIRECTION('center_axis',(0.,-1.,0.));
#5767=DIRECTION('ref_axis',(1.,0.,0.));
#5768=DIRECTION('center_axis',(0.866025403784439,0.,-0.5));
#5769=DIRECTION('ref_axis',(-0.5,0.,-0.866025403784439));
#5770=DIRECTION('',(0.866025403784439,0.,-0.5));
#5771=DIRECTION('center_axis',(0.866025403784439,0.,-0.5));
#5772=DIRECTION('ref_axis',(-0.5,0.,-0.866025403784439));
#5773=DIRECTION('',(0.866025403784439,0.,-0.5));
#5774=DIRECTION('center_axis',(0.,0.,1.));
#5775=DIRECTION('ref_axis',(1.,0.,0.));
#5776=DIRECTION('',(0.,0.,1.));
#5777=DIRECTION('center_axis',(0.,0.,1.));
#5778=DIRECTION('ref_axis',(1.,0.,0.));
#5779=DIRECTION('',(0.,0.,1.));
#5780=DIRECTION('center_axis',(0.,1.,0.));
#5781=DIRECTION('ref_axis',(0.,0.,1.));
#5782=DIRECTION('center_axis',(0.,-1.,0.));
#5783=DIRECTION('ref_axis',(1.,0.,0.));
#5784=DIRECTION('center_axis',(0.,1.,0.));
#5785=DIRECTION('ref_axis',(0.,0.,1.));
#5786=DIRECTION('center_axis',(0.,-1.,0.));
#5787=DIRECTION('ref_axis',(1.,0.,0.));
#5788=DIRECTION('center_axis',(0.,-1.,0.));
#5789=DIRECTION('ref_axis',(1.,0.,0.));
#5790=DIRECTION('center_axis',(0.,-1.,0.));
#5791=DIRECTION('ref_axis',(1.,0.,0.));
#5792=DIRECTION('',(0.,1.,0.));
#5793=DIRECTION('center_axis',(0.,-1.,0.));
#5794=DIRECTION('ref_axis',(0.,0.,-1.));
#5795=DIRECTION('center_axis',(0.,-1.,0.));
#5796=DIRECTION('ref_axis',(1.,0.,0.));
#5797=DIRECTION('center_axis',(0.,-1.,0.));
#5798=DIRECTION('ref_axis',(1.,0.,0.));
#5799=DIRECTION('',(0.,1.,0.));
#5800=DIRECTION('',(0.,0.,1.));
#5801=DIRECTION('',(1.,0.,0.));
#5802=DIRECTION('',(0.,0.,1.));
#5803=DIRECTION('',(1.,0.,0.));
#5804=DIRECTION('axis',(0.,0.,1.));
#5805=DIRECTION('refdir',(1.,0.,0.));
#5806=DIRECTION('center_axis',(0.,1.,0.));
#5807=DIRECTION('ref_axis',(1.,0.,0.));
#5808=DIRECTION('center_axis',(0.,-1.,0.));
#5809=DIRECTION('ref_axis',(1.,0.,0.));
#5810=DIRECTION('',(0.,-1.,0.));
#5811=DIRECTION('center_axis',(0.,-1.,0.));
#5812=DIRECTION('ref_axis',(1.,0.,0.));
#5813=DIRECTION('center_axis',(0.,1.,0.));
#5814=DIRECTION('ref_axis',(1.,0.,0.));
#5815=DIRECTION('center_axis',(0.,1.,0.));
#5816=DIRECTION('ref_axis',(1.,0.,0.));
#5817=DIRECTION('',(0.,-1.,0.));
#5818=DIRECTION('center_axis',(0.,1.,0.));
#5819=DIRECTION('ref_axis',(1.,0.,0.));
#5820=DIRECTION('center_axis',(0.,1.,0.));
#5821=DIRECTION('ref_axis',(1.,0.,0.));
#5822=DIRECTION('center_axis',(0.,1.,0.));
#5823=DIRECTION('ref_axis',(1.,0.,0.));
#5824=DIRECTION('axis',(0.,0.,1.));
#5825=DIRECTION('refdir',(1.,0.,0.));
#5826=DIRECTION('center_axis',(0.866025403784439,0.,-0.5));
#5827=DIRECTION('ref_axis',(0.5,0.,0.866025403784439));
#5828=DIRECTION('',(-0.5,0.,-0.866025403784439));
#5829=DIRECTION('',(0.,-1.,0.));
#5830=DIRECTION('',(0.5,0.,0.866025403784439));
#5831=DIRECTION('',(0.,-1.,0.));
#5832=DIRECTION('center_axis',(1.60246890531964E-16,0.,-1.));
#5833=DIRECTION('ref_axis',(1.,0.,1.60246890531964E-16));
#5834=DIRECTION('',(-1.,0.,-1.60246890531964E-16));
#5835=DIRECTION('',(0.,-1.,0.));
#5836=DIRECTION('',(1.,0.,1.60246890531964E-16));
#5837=DIRECTION('center_axis',(-0.866025403784439,0.,-0.5));
#5838=DIRECTION('ref_axis',(0.5,0.,-0.866025403784439));
#5839=DIRECTION('',(-0.5,0.,0.866025403784439));
#5840=DIRECTION('',(0.,-1.,0.));
#5841=DIRECTION('',(0.5,0.,-0.866025403784439));
#5842=DIRECTION('center_axis',(-0.866025403784439,0.,0.5));
#5843=DIRECTION('ref_axis',(-0.5,0.,-0.866025403784439));
#5844=DIRECTION('',(0.5,0.,0.866025403784439));
#5845=DIRECTION('',(0.,-1.,0.));
#5846=DIRECTION('',(-0.5,0.,-0.866025403784439));
#5847=DIRECTION('center_axis',(-1.60246890531964E-16,0.,1.));
#5848=DIRECTION('ref_axis',(-1.,0.,-1.60246890531964E-16));
#5849=DIRECTION('',(1.,0.,1.60246890531964E-16));
#5850=DIRECTION('',(0.,-1.,0.));
#5851=DIRECTION('',(-1.,0.,-1.60246890531964E-16));
#5852=DIRECTION('center_axis',(0.866025403784439,0.,0.5));
#5853=DIRECTION('ref_axis',(-0.5,0.,0.866025403784439));
#5854=DIRECTION('',(0.5,0.,-0.866025403784439));
#5855=DIRECTION('',(-0.5,0.,0.866025403784439));
#5856=DIRECTION('center_axis',(0.,1.,0.));
#5857=DIRECTION('ref_axis',(1.,0.,0.));
#5858=DIRECTION('center_axis',(0.,-1.,0.));
#5859=DIRECTION('ref_axis',(0.,0.,-1.));
#5860=DIRECTION('center_axis',(0.,1.,0.));
#5861=DIRECTION('ref_axis',(1.,0.,0.));
#5862=DIRECTION('center_axis',(0.,1.,0.));
#5863=DIRECTION('ref_axis',(1.,0.,0.));
#5864=DIRECTION('center_axis',(0.,1.,0.));
#5865=DIRECTION('ref_axis',(0.,0.,1.));
#5866=DIRECTION('center_axis',(0.,-1.,0.));
#5867=DIRECTION('ref_axis',(1.,0.,0.));
#5868=DIRECTION('center_axis',(0.,-1.,0.));
#5869=DIRECTION('ref_axis',(1.,0.,0.));
#5870=DIRECTION('center_axis',(0.,-1.,0.));
#5871=DIRECTION('ref_axis',(1.,0.,0.));
#5872=DIRECTION('',(0.707106781186548,0.707106781186547,8.65956056235493E-17));
#5873=DIRECTION('center_axis',(0.,-1.,0.));
#5874=DIRECTION('ref_axis',(1.,0.,0.));
#5875=DIRECTION('center_axis',(0.,-1.,0.));
#5876=DIRECTION('ref_axis',(1.,0.,0.));
#5877=DIRECTION('',(0.,1.,0.));
#5878=DIRECTION('center_axis',(0.,1.,0.));
#5879=DIRECTION('ref_axis',(1.,0.,0.));
#5880=DIRECTION('center_axis',(0.,-1.,0.));
#5881=DIRECTION('ref_axis',(1.,0.,0.));
#5882=DIRECTION('',(-0.707106781186548,0.707106781186547,-8.65956056235494E-17));
#5883=DIRECTION('center_axis',(0.,-1.,0.));
#5884=DIRECTION('ref_axis',(0.,0.,-1.));
#5885=DIRECTION('center_axis',(0.,-1.,0.));
#5886=DIRECTION('ref_axis',(1.,0.,0.));
#5887=DIRECTION('center_axis',(0.,1.,0.));
#5888=DIRECTION('ref_axis',(1.,0.,0.));
#5889=DIRECTION('center_axis',(0.,1.,0.));
#5890=DIRECTION('ref_axis',(1.,0.,0.));
#5891=DIRECTION('',(-0.447213595499958,0.894427190999916,-5.47678698264203E-17));
#5892=DIRECTION('center_axis',(0.,-1.,0.));
#5893=DIRECTION('ref_axis',(1.,0.,0.));
#5894=DIRECTION('',(0.,1.,0.));
#5895=DIRECTION('',(0.,0.,1.));
#5896=DIRECTION('',(1.,0.,0.));
#5897=DIRECTION('',(0.,0.,1.));
#5898=DIRECTION('',(1.,0.,0.));
#5899=DIRECTION('',(0.,0.,1.));
#5900=DIRECTION('',(1.,0.,0.));
#5901=DIRECTION('',(0.,0.,1.));
#5902=DIRECTION('',(1.,0.,0.));
#5903=DIRECTION('',(0.,0.,1.));
#5904=DIRECTION('',(1.,0.,0.));
#5905=DIRECTION('',(0.,0.,1.));
#5906=DIRECTION('',(1.,0.,0.));
#5907=DIRECTION('',(0.,0.,1.));
#5908=DIRECTION('',(1.,0.,0.));
#5909=DIRECTION('',(0.,0.,1.));
#5910=DIRECTION('',(1.,0.,0.));
#5911=DIRECTION('',(0.,0.,1.));
#5912=DIRECTION('',(1.,0.,0.));
#5913=DIRECTION('',(0.,0.,1.));
#5914=DIRECTION('',(1.,0.,0.));
#5915=DIRECTION('',(0.,0.,1.));
#5916=DIRECTION('',(1.,0.,0.));
#5917=DIRECTION('',(0.,-1.,2.22044604925031E-16));
#5918=DIRECTION('',(1.,0.,0.));
#5919=DIRECTION('',(0.,-1.,2.22044604925031E-16));
#5920=DIRECTION('',(1.,0.,0.));
#5921=DIRECTION('',(0.,-1.,2.22044604925031E-16));
#5922=DIRECTION('',(1.,0.,0.));
#5923=DIRECTION('',(0.,-1.,2.22044604925031E-16));
#5924=DIRECTION('',(1.,0.,0.));
#5925=DIRECTION('',(0.,-1.,2.22044604925031E-16));
#5926=DIRECTION('',(1.,0.,0.));
#5927=DIRECTION('',(0.,-1.,2.22044604925031E-16));
#5928=DIRECTION('',(1.,0.,0.));
#5929=DIRECTION('',(0.,-1.,2.22044604925031E-16));
#5930=DIRECTION('',(1.,0.,0.));
#5931=DIRECTION('',(0.,-1.,2.22044604925031E-16));
#5932=DIRECTION('',(1.,0.,0.));
#5933=DIRECTION('',(0.,0.,1.));
#5934=DIRECTION('',(1.,0.,0.));
#5935=DIRECTION('',(0.,-1.,2.22044604925031E-16));
#5936=DIRECTION('',(1.,0.,0.));
#5937=DIRECTION('',(0.,-1.,2.22044604925031E-16));
#5938=DIRECTION('',(1.,0.,0.));
#5939=DIRECTION('',(0.,-1.,2.22044604925031E-16));
#5940=DIRECTION('',(1.,0.,0.));
#5941=DIRECTION('',(0.,-1.,2.22044604925031E-16));
#5942=DIRECTION('',(1.,0.,0.));
#5943=DIRECTION('',(0.,0.,1.));
#5944=DIRECTION('',(1.,0.,0.));
#5945=DIRECTION('',(0.,-1.,2.22044604925031E-16));
#5946=DIRECTION('',(1.,0.,0.));
#5947=DIRECTION('',(0.,-1.,2.22044604925031E-16));
#5948=DIRECTION('',(1.,0.,0.));
#5949=DIRECTION('',(0.,-1.,2.22044604925031E-16));
#5950=DIRECTION('',(1.,0.,0.));
#5951=DIRECTION('',(0.,-1.,2.22044604925031E-16));
#5952=DIRECTION('',(1.,0.,0.));
#5953=DIRECTION('',(0.,0.,1.));
#5954=DIRECTION('',(1.,0.,0.));
#5955=DIRECTION('',(0.,-1.,2.22044604925031E-16));
#5956=DIRECTION('',(1.,0.,0.));
#5957=DIRECTION('',(0.,-1.,2.22044604925031E-16));
#5958=DIRECTION('',(1.,0.,0.));
#5959=DIRECTION('',(0.,-1.,2.22044604925031E-16));
#5960=DIRECTION('',(1.,0.,0.));
#5961=DIRECTION('',(0.,-1.,2.22044604925031E-16));
#5962=DIRECTION('',(1.,0.,0.));
#5963=DIRECTION('axis',(0.,0.,1.));
#5964=DIRECTION('refdir',(1.,0.,0.));
#5965=DIRECTION('axis',(0.,0.,1.));
#5966=DIRECTION('refdir',(1.,0.,0.));
#5967=DIRECTION('center_axis',(0.,1.,0.));
#5968=DIRECTION('ref_axis',(1.,0.,0.));
#5969=DIRECTION('center_axis',(0.,1.,0.));
#5970=DIRECTION('ref_axis',(1.,0.,0.));
#5971=DIRECTION('',(0.,1.,0.));
#5972=DIRECTION('center_axis',(0.,-1.,0.));
#5973=DIRECTION('ref_axis',(1.,0.,0.));
#5974=DIRECTION('center_axis',(0.,1.,0.));
#5975=DIRECTION('ref_axis',(1.,0.,0.));
#5976=DIRECTION('center_axis',(0.,1.,0.));
#5977=DIRECTION('ref_axis',(1.,0.,0.));
#5978=DIRECTION('center_axis',(0.,1.,0.));
#5979=DIRECTION('ref_axis',(1.,0.,0.));
#5980=DIRECTION('',(0.,1.,0.));
#5981=DIRECTION('center_axis',(0.,1.,0.));
#5982=DIRECTION('ref_axis',(1.,0.,0.));
#5983=DIRECTION('center_axis',(0.,1.,0.));
#5984=DIRECTION('ref_axis',(1.,0.,0.));
#5985=DIRECTION('center_axis',(-1.,0.,0.));
#5986=DIRECTION('ref_axis',(0.,0.,1.));
#5987=DIRECTION('',(0.,-1.,0.));
#5988=DIRECTION('',(0.,0.,1.));
#5989=DIRECTION('',(0.,1.,0.));
#5990=DIRECTION('',(0.,0.,-1.));
#5991=DIRECTION('center_axis',(0.,1.,0.));
#5992=DIRECTION('ref_axis',(1.,0.,0.));
#5993=DIRECTION('center_axis',(0.,-1.,0.));
#5994=DIRECTION('ref_axis',(1.,0.,0.));
#5995=DIRECTION('',(-1.,0.,0.));
#5996=DIRECTION('',(0.,0.,1.));
#5997=DIRECTION('center_axis',(1.,0.,0.));
#5998=DIRECTION('ref_axis',(0.,0.,-1.));
#5999=DIRECTION('',(0.,1.,0.));
#6000=DIRECTION('',(0.,1.,0.));
#6001=DIRECTION('',(0.,0.,-1.));
#6002=DIRECTION('center_axis',(0.,0.,1.));
#6003=DIRECTION('ref_axis',(1.,0.,0.));
#6004=DIRECTION('',(1.,0.,0.));
#6005=DIRECTION('center_axis',(0.,1.,0.));
#6006=DIRECTION('ref_axis',(0.,0.,1.));
#6007=DIRECTION('center_axis',(0.,1.,0.));
#6008=DIRECTION('ref_axis',(1.,0.,0.));
#6009=DIRECTION('center_axis',(-1.,0.,0.));
#6010=DIRECTION('ref_axis',(0.,0.,1.));
#6011=DIRECTION('',(0.,-1.,0.));
#6012=DIRECTION('',(0.,0.,1.));
#6013=DIRECTION('',(0.,1.,0.));
#6014=DIRECTION('',(0.,0.,-1.));
#6015=DIRECTION('center_axis',(0.,1.,0.));
#6016=DIRECTION('ref_axis',(1.,0.,0.));
#6017=DIRECTION('center_axis',(0.,-1.,0.));
#6018=DIRECTION('ref_axis',(1.,0.,0.));
#6019=DIRECTION('',(-1.,0.,0.));
#6020=DIRECTION('',(0.,0.,1.));
#6021=DIRECTION('center_axis',(1.,0.,0.));
#6022=DIRECTION('ref_axis',(0.,0.,-1.));
#6023=DIRECTION('',(0.,1.,0.));
#6024=DIRECTION('',(0.,1.,0.));
#6025=DIRECTION('',(0.,0.,-1.));
#6026=DIRECTION('center_axis',(0.,0.,1.));
#6027=DIRECTION('ref_axis',(1.,0.,0.));
#6028=DIRECTION('',(1.,0.,0.));
#6029=DIRECTION('center_axis',(0.,1.,0.));
#6030=DIRECTION('ref_axis',(0.,0.,1.));
#6031=DIRECTION('center_axis',(0.,1.,0.));
#6032=DIRECTION('ref_axis',(1.,0.,0.));
#6033=DIRECTION('center_axis',(0.,1.,0.));
#6034=DIRECTION('ref_axis',(1.,0.,0.));
#6035=DIRECTION('center_axis',(0.,1.,0.));
#6036=DIRECTION('ref_axis',(1.,0.,0.));
#6037=DIRECTION('',(0.,-1.,0.));
#6038=DIRECTION('center_axis',(0.,1.,0.));
#6039=DIRECTION('ref_axis',(1.,0.,0.));
#6040=DIRECTION('center_axis',(0.,1.,0.));
#6041=DIRECTION('ref_axis',(1.,0.,0.));
#6042=DIRECTION('center_axis',(0.,1.,0.));
#6043=DIRECTION('ref_axis',(1.,0.,0.));
#6044=DIRECTION('axis',(0.,0.,1.));
#6045=DIRECTION('refdir',(1.,0.,0.));
#6046=DIRECTION('center_axis',(0.,0.,1.));
#6047=DIRECTION('ref_axis',(1.,0.,0.));
#6048=DIRECTION('',(0.,1.,0.));
#6049=DIRECTION('center_axis',(0.,0.,1.));
#6050=DIRECTION('ref_axis',(1.,0.,0.));
#6051=DIRECTION('center_axis',(0.,0.,1.));
#6052=DIRECTION('ref_axis',(1.,0.,0.));
#6053=DIRECTION('center_axis',(0.,0.,1.));
#6054=DIRECTION('ref_axis',(1.,0.,0.));
#6055=DIRECTION('',(0.,0.,1.));
#6056=DIRECTION('center_axis',(0.,0.,1.));
#6057=DIRECTION('ref_axis',(1.,0.,0.));
#6058=DIRECTION('center_axis',(0.,0.,1.));
#6059=DIRECTION('ref_axis',(1.,0.,0.));
#6060=DIRECTION('',(0.,-1.,0.));
#6061=DIRECTION('center_axis',(-1.,0.,0.));
#6062=DIRECTION('ref_axis',(0.,0.,1.));
#6063=DIRECTION('',(0.,0.,1.));
#6064=DIRECTION('',(0.,1.,0.));
#6065=DIRECTION('',(0.,0.,-1.));
#6066=DIRECTION('',(0.,1.,0.));
#6067=DIRECTION('center_axis',(0.,0.,-1.));
#6068=DIRECTION('ref_axis',(-1.,0.,0.));
#6069=DIRECTION('',(-1.,0.,0.));
#6070=DIRECTION('',(0.,1.,0.));
#6071=DIRECTION('',(1.,0.,0.));
#6072=DIRECTION('center_axis',(1.,0.,0.));
#6073=DIRECTION('ref_axis',(0.,0.,-1.));
#6074=DIRECTION('',(0.,0.,-1.));
#6075=DIRECTION('',(0.,-1.,0.));
#6076=DIRECTION('',(0.,0.,1.));
#6077=DIRECTION('center_axis',(0.,1.,0.));
#6078=DIRECTION('ref_axis',(1.,0.,0.));
#6079=DIRECTION('center_axis',(0.,1.,0.));
#6080=DIRECTION('ref_axis',(1.,0.,0.));
#6081=DIRECTION('center_axis',(0.,-1.,0.));
#6082=DIRECTION('ref_axis',(1.,0.,0.));
#6083=DIRECTION('center_axis',(0.,1.,0.));
#6084=DIRECTION('ref_axis',(-1.83697019872103E-16,0.,1.));
#6085=DIRECTION('center_axis',(0.,-1.,0.));
#6086=DIRECTION('ref_axis',(1.,0.,0.));
#6087=DIRECTION('center_axis',(0.,1.,0.));
#6088=DIRECTION('ref_axis',(1.,0.,0.));
#6089=DIRECTION('',(0.,-1.,0.));
#6090=DIRECTION('center_axis',(0.,1.,0.));
#6091=DIRECTION('ref_axis',(1.,0.,0.));
#6092=DIRECTION('center_axis',(0.,1.,0.));
#6093=DIRECTION('ref_axis',(1.,0.,0.));
#6094=DIRECTION('axis',(0.,0.,1.));
#6095=DIRECTION('refdir',(1.,0.,0.));
#6096=DIRECTION('center_axis',(0.,0.,1.));
#6097=DIRECTION('ref_axis',(1.,0.,0.));
#6098=DIRECTION('',(0.,1.,0.));
#6099=DIRECTION('center_axis',(0.,0.,1.));
#6100=DIRECTION('ref_axis',(1.,0.,0.));
#6101=DIRECTION('center_axis',(0.,0.,1.));
#6102=DIRECTION('ref_axis',(1.,0.,0.));
#6103=DIRECTION('center_axis',(0.,0.,1.));
#6104=DIRECTION('ref_axis',(1.,0.,0.));
#6105=DIRECTION('',(0.,0.,1.));
#6106=DIRECTION('center_axis',(0.,0.,1.));
#6107=DIRECTION('ref_axis',(1.,0.,0.));
#6108=DIRECTION('center_axis',(0.,0.,1.));
#6109=DIRECTION('ref_axis',(1.,0.,0.));
#6110=DIRECTION('',(0.,-1.,0.));
#6111=DIRECTION('center_axis',(-1.,0.,0.));
#6112=DIRECTION('ref_axis',(0.,0.,1.));
#6113=DIRECTION('',(0.,0.,1.));
#6114=DIRECTION('',(0.,1.,0.));
#6115=DIRECTION('',(0.,0.,-1.));
#6116=DIRECTION('',(0.,1.,0.));
#6117=DIRECTION('center_axis',(0.,0.,-1.));
#6118=DIRECTION('ref_axis',(-1.,0.,0.));
#6119=DIRECTION('',(-1.,0.,0.));
#6120=DIRECTION('',(0.,1.,0.));
#6121=DIRECTION('',(1.,0.,0.));
#6122=DIRECTION('center_axis',(1.,0.,0.));
#6123=DIRECTION('ref_axis',(0.,0.,-1.));
#6124=DIRECTION('',(0.,0.,-1.));
#6125=DIRECTION('',(0.,-1.,0.));
#6126=DIRECTION('',(0.,0.,1.));
#6127=DIRECTION('center_axis',(0.,1.,0.));
#6128=DIRECTION('ref_axis',(1.,0.,0.));
#6129=DIRECTION('center_axis',(0.,1.,0.));
#6130=DIRECTION('ref_axis',(1.,0.,0.));
#6131=DIRECTION('center_axis',(0.,-1.,0.));
#6132=DIRECTION('ref_axis',(1.,0.,0.));
#6133=DIRECTION('center_axis',(0.,1.,0.));
#6134=DIRECTION('ref_axis',(-1.83697019872103E-16,0.,1.));
#6135=DIRECTION('center_axis',(0.,-1.,0.));
#6136=DIRECTION('ref_axis',(1.,0.,0.));
#6137=DIRECTION('center_axis',(0.,1.,0.));
#6138=DIRECTION('ref_axis',(1.,0.,0.));
#6139=DIRECTION('',(0.,-1.,0.));
#6140=DIRECTION('center_axis',(0.,1.,0.));
#6141=DIRECTION('ref_axis',(1.,0.,0.));
#6142=DIRECTION('center_axis',(0.,1.,0.));
#6143=DIRECTION('ref_axis',(1.,0.,0.));
#6144=DIRECTION('axis',(0.,0.,1.));
#6145=DIRECTION('refdir',(1.,0.,0.));
#6146=DIRECTION('center_axis',(0.,0.,1.));
#6147=DIRECTION('ref_axis',(1.,0.,0.));
#6148=DIRECTION('',(0.,1.,0.));
#6149=DIRECTION('center_axis',(0.,0.,1.));
#6150=DIRECTION('ref_axis',(1.,0.,0.));
#6151=DIRECTION('center_axis',(0.,0.,1.));
#6152=DIRECTION('ref_axis',(1.,0.,0.));
#6153=DIRECTION('center_axis',(0.,0.,1.));
#6154=DIRECTION('ref_axis',(1.,0.,0.));
#6155=DIRECTION('',(0.,0.,1.));
#6156=DIRECTION('center_axis',(0.,0.,1.));
#6157=DIRECTION('ref_axis',(1.,0.,0.));
#6158=DIRECTION('center_axis',(0.,0.,1.));
#6159=DIRECTION('ref_axis',(1.,0.,0.));
#6160=DIRECTION('',(0.,-1.,0.));
#6161=DIRECTION('center_axis',(0.,1.,0.));
#6162=DIRECTION('ref_axis',(1.,0.,0.));
#6163=DIRECTION('center_axis',(0.,-1.,0.));
#6164=DIRECTION('ref_axis',(1.,0.,0.));
#6165=DIRECTION('',(0.,-1.,0.));
#6166=DIRECTION('center_axis',(0.,-1.,0.));
#6167=DIRECTION('ref_axis',(1.,0.,0.));
#6168=DIRECTION('center_axis',(0.,1.,0.));
#6169=DIRECTION('ref_axis',(1.,0.,0.));
#6170=DIRECTION('center_axis',(0.,1.,0.));
#6171=DIRECTION('ref_axis',(1.,0.,0.));
#6172=DIRECTION('',(0.,-1.,0.));
#6173=DIRECTION('center_axis',(0.,1.,0.));
#6174=DIRECTION('ref_axis',(1.,0.,0.));
#6175=DIRECTION('center_axis',(0.,1.,0.));
#6176=DIRECTION('ref_axis',(1.,0.,0.));
#6177=DIRECTION('center_axis',(0.,1.,0.));
#6178=DIRECTION('ref_axis',(1.,0.,0.));
#6179=DIRECTION('axis',(0.,0.,1.));
#6180=DIRECTION('refdir',(1.,0.,0.));
#6181=DIRECTION('center_axis',(0.,0.,1.));
#6182=DIRECTION('ref_axis',(1.,0.,0.));
#6183=DIRECTION('',(0.,1.,0.));
#6184=DIRECTION('center_axis',(0.,0.,1.));
#6185=DIRECTION('ref_axis',(1.,0.,0.));
#6186=DIRECTION('center_axis',(0.,0.,1.));
#6187=DIRECTION('ref_axis',(1.,0.,0.));
#6188=DIRECTION('center_axis',(0.,0.,1.));
#6189=DIRECTION('ref_axis',(1.,0.,0.));
#6190=DIRECTION('',(0.,0.,1.));
#6191=DIRECTION('center_axis',(0.,0.,1.));
#6192=DIRECTION('ref_axis',(1.,0.,0.));
#6193=DIRECTION('center_axis',(0.,0.,1.));
#6194=DIRECTION('ref_axis',(1.,0.,0.));
#6195=DIRECTION('',(0.,-1.,0.));
#6196=DIRECTION('center_axis',(0.,1.,0.));
#6197=DIRECTION('ref_axis',(1.,0.,0.));
#6198=DIRECTION('center_axis',(0.,-1.,0.));
#6199=DIRECTION('ref_axis',(1.,0.,0.));
#6200=DIRECTION('',(0.,-1.,0.));
#6201=DIRECTION('center_axis',(0.,-1.,0.));
#6202=DIRECTION('ref_axis',(1.,0.,0.));
#6203=DIRECTION('center_axis',(0.,1.,0.));
#6204=DIRECTION('ref_axis',(1.,0.,0.));
#6205=DIRECTION('center_axis',(0.,1.,0.));
#6206=DIRECTION('ref_axis',(1.,0.,0.));
#6207=DIRECTION('',(0.,-1.,0.));
#6208=DIRECTION('center_axis',(0.,1.,0.));
#6209=DIRECTION('ref_axis',(1.,0.,0.));
#6210=DIRECTION('center_axis',(0.,1.,0.));
#6211=DIRECTION('ref_axis',(1.,0.,0.));
#6212=DIRECTION('center_axis',(0.,1.,0.));
#6213=DIRECTION('ref_axis',(1.,0.,0.));
#6214=DIRECTION('axis',(0.,0.,1.));
#6215=DIRECTION('refdir',(1.,0.,0.));
#6216=DIRECTION('center_axis',(0.,1.,0.));
#6217=DIRECTION('ref_axis',(1.,0.,0.));
#6218=DIRECTION('center_axis',(0.,-1.,0.));
#6219=DIRECTION('ref_axis',(1.,0.,0.));
#6220=DIRECTION('',(0.,-1.,0.));
#6221=DIRECTION('center_axis',(0.,-1.,0.));
#6222=DIRECTION('ref_axis',(1.,0.,0.));
#6223=DIRECTION('center_axis',(0.,1.,0.));
#6224=DIRECTION('ref_axis',(1.,0.,0.));
#6225=DIRECTION('center_axis',(0.,1.,0.));
#6226=DIRECTION('ref_axis',(1.,0.,0.));
#6227=DIRECTION('',(0.,-1.,0.));
#6228=DIRECTION('center_axis',(0.,1.,0.));
#6229=DIRECTION('ref_axis',(1.,0.,0.));
#6230=DIRECTION('center_axis',(0.,1.,0.));
#6231=DIRECTION('ref_axis',(1.,0.,0.));
#6232=DIRECTION('center_axis',(0.,1.,0.));
#6233=DIRECTION('ref_axis',(1.,0.,0.));
#6234=DIRECTION('axis',(0.,0.,1.));
#6235=DIRECTION('refdir',(1.,0.,0.));
#6236=DIRECTION('center_axis',(0.,1.,0.));
#6237=DIRECTION('ref_axis',(1.,0.,0.));
#6238=DIRECTION('center_axis',(0.,-1.,0.));
#6239=DIRECTION('ref_axis',(1.,0.,0.));
#6240=DIRECTION('',(0.,-1.,0.));
#6241=DIRECTION('center_axis',(0.,-1.,0.));
#6242=DIRECTION('ref_axis',(1.,0.,0.));
#6243=DIRECTION('center_axis',(0.,1.,0.));
#6244=DIRECTION('ref_axis',(1.,0.,0.));
#6245=DIRECTION('center_axis',(0.,1.,0.));
#6246=DIRECTION('ref_axis',(1.,0.,0.));
#6247=DIRECTION('',(0.,-1.,0.));
#6248=DIRECTION('center_axis',(0.,1.,0.));
#6249=DIRECTION('ref_axis',(1.,0.,0.));
#6250=DIRECTION('center_axis',(0.,1.,0.));
#6251=DIRECTION('ref_axis',(1.,0.,0.));
#6252=DIRECTION('center_axis',(0.,1.,0.));
#6253=DIRECTION('ref_axis',(1.,0.,0.));
#6254=DIRECTION('axis',(0.,0.,1.));
#6255=DIRECTION('refdir',(1.,0.,0.));
#6256=DIRECTION('center_axis',(1.,0.,0.));
#6257=DIRECTION('ref_axis',(0.,0.,-1.));
#6258=DIRECTION('',(0.,-0.707106781186547,-0.707106781186548));
#6259=DIRECTION('',(0.,-1.,0.));
#6260=DIRECTION('',(0.,-0.707106781186547,0.707106781186548));
#6261=DIRECTION('',(0.,0.,1.));
#6262=DIRECTION('',(0.,0.707106781186547,0.707106781186548));
#6263=DIRECTION('',(0.,1.,0.));
#6264=DIRECTION('',(0.,0.707106781186547,-0.707106781186548));
#6265=DIRECTION('',(0.,0.,-1.));
#6266=DIRECTION('center_axis',(0.,0.707106781186548,-0.707106781186547));
#6267=DIRECTION('ref_axis',(-1.,0.,0.));
#6268=DIRECTION('',(1.,0.,0.));
#6269=DIRECTION('',(0.,-0.707106781186547,-0.707106781186548));
#6270=DIRECTION('',(-1.,0.,0.));
#6271=DIRECTION('center_axis',(0.,1.,0.));
#6272=DIRECTION('ref_axis',(-1.,0.,0.));
#6273=DIRECTION('',(-1.,0.,0.));
#6274=DIRECTION('',(0.,0.,-1.));
#6275=DIRECTION('center_axis',(0.,0.707106781186548,0.707106781186547));
#6276=DIRECTION('ref_axis',(1.,0.,0.));
#6277=DIRECTION('',(1.,0.,0.));
#6278=DIRECTION('',(0.,0.707106781186547,-0.707106781186548));
#6279=DIRECTION('center_axis',(0.,0.,1.));
#6280=DIRECTION('ref_axis',(1.,0.,0.));
#6281=DIRECTION('',(-1.,0.,0.));
#6282=DIRECTION('',(0.,1.,0.));
#6283=DIRECTION('center_axis',(1.,0.,0.));
#6284=DIRECTION('ref_axis',(0.,0.,-1.));
#6285=DIRECTION('',(0.,-0.707106781186547,0.707106781186548));
#6286=DIRECTION('',(0.,-1.,0.));
#6287=DIRECTION('',(0.,0.707106781186547,0.707106781186548));
#6288=DIRECTION('',(0.,0.,1.));
#6289=DIRECTION('center_axis',(0.,0.,1.));
#6290=DIRECTION('ref_axis',(1.,0.,0.));
#6291=DIRECTION('',(1.,0.,0.));
#6292=DIRECTION('center_axis',(0.,-0.707106781186548,0.707106781186547));
#6293=DIRECTION('ref_axis',(1.,0.,0.));
#6294=DIRECTION('',(1.,0.,0.));
#6295=DIRECTION('center_axis',(0.,-0.707106781186548,-0.707106781186547));
#6296=DIRECTION('ref_axis',(-1.,0.,0.));
#6297=DIRECTION('',(-1.,0.,0.));
#6298=DIRECTION('center_axis',(0.,-1.,0.));
#6299=DIRECTION('ref_axis',(1.,0.,0.));
#6300=DIRECTION('axis',(0.,0.,1.));
#6301=DIRECTION('refdir',(1.,0.,0.));
#6302=DIRECTION('center_axis',(0.866025403784439,0.,-0.5));
#6303=DIRECTION('ref_axis',(0.5,0.,0.866025403784439));
#6304=DIRECTION('',(0.5,0.,0.866025403784439));
#6305=DIRECTION('',(0.,-1.,0.));
#6306=DIRECTION('',(0.5,0.,0.866025403784439));
#6307=DIRECTION('',(0.,-1.,0.));
#6308=DIRECTION('center_axis',(1.92296268638356E-16,0.,-1.));
#6309=DIRECTION('ref_axis',(1.,0.,1.92296268638356E-16));
#6310=DIRECTION('',(1.,0.,1.92296268638356E-16));
#6311=DIRECTION('',(0.,-1.,0.));
#6312=DIRECTION('',(1.,0.,1.92296268638356E-16));
#6313=DIRECTION('center_axis',(-0.866025403784439,0.,-0.5));
#6314=DIRECTION('ref_axis',(0.5,0.,-0.866025403784439));
#6315=DIRECTION('',(0.5,0.,-0.866025403784439));
#6316=DIRECTION('',(0.,-1.,0.));
#6317=DIRECTION('',(0.5,0.,-0.866025403784438));
#6318=DIRECTION('center_axis',(-0.866025403784439,0.,0.5));
#6319=DIRECTION('ref_axis',(-0.5,0.,-0.866025403784439));
#6320=DIRECTION('',(-0.5,0.,-0.866025403784439));
#6321=DIRECTION('',(0.,-1.,0.));
#6322=DIRECTION('',(-0.5,0.,-0.866025403784439));
#6323=DIRECTION('center_axis',(-1.92296268638356E-16,0.,1.));
#6324=DIRECTION('ref_axis',(-1.,0.,-1.92296268638356E-16));
#6325=DIRECTION('',(-1.,0.,-1.92296268638356E-16));
#6326=DIRECTION('',(0.,-1.,0.));
#6327=DIRECTION('',(-1.,0.,-1.92296268638356E-16));
#6328=DIRECTION('center_axis',(0.866025403784439,0.,0.5));
#6329=DIRECTION('ref_axis',(-0.5,0.,0.866025403784439));
#6330=DIRECTION('',(-0.5,0.,0.866025403784439));
#6331=DIRECTION('',(-0.5,0.,0.866025403784439));
#6332=DIRECTION('center_axis',(0.,-1.,0.));
#6333=DIRECTION('ref_axis',(0.,0.,-1.));
#6334=DIRECTION('center_axis',(0.,1.,0.));
#6335=DIRECTION('ref_axis',(0.,0.,1.));
#6336=DIRECTION('center_axis',(0.,-1.,0.));
#6337=DIRECTION('ref_axis',(1.,0.,0.));
#6338=DIRECTION('center_axis',(0.,-1.,0.));
#6339=DIRECTION('ref_axis',(1.,0.,0.));
#6340=DIRECTION('center_axis',(0.,-1.,0.));
#6341=DIRECTION('ref_axis',(1.,0.,0.));
#6342=DIRECTION('',(0.707106781186547,0.707106781186548,8.65956056235493E-17));
#6343=DIRECTION('center_axis',(0.,-1.,0.));
#6344=DIRECTION('ref_axis',(1.,0.,0.));
#6345=DIRECTION('center_axis',(0.,1.,0.));
#6346=DIRECTION('ref_axis',(1.,0.,0.));
#6347=DIRECTION('',(0.,1.,0.));
#6348=DIRECTION('center_axis',(0.,1.,0.));
#6349=DIRECTION('ref_axis',(1.,0.,0.));
#6350=DIRECTION('center_axis',(0.,-1.,0.));
#6351=DIRECTION('ref_axis',(1.,0.,0.));
#6352=DIRECTION('',(-0.707106781186547,0.707106781186548,-8.65956056235493E-17));
#6353=DIRECTION('center_axis',(0.,-1.,0.));
#6354=DIRECTION('ref_axis',(0.,0.,-1.));
#6355=DIRECTION('axis',(0.,0.,1.));
#6356=DIRECTION('refdir',(1.,0.,0.));
#6357=DIRECTION('center_axis',(0.,1.,0.));
#6358=DIRECTION('ref_axis',(0.,0.,1.));
#6359=DIRECTION('center_axis',(0.,-1.,0.));
#6360=DIRECTION('ref_axis',(1.,0.,0.));
#6361=DIRECTION('center_axis',(0.,-1.,0.));
#6362=DIRECTION('ref_axis',(1.,0.,0.));
#6363=DIRECTION('center_axis',(0.,-1.,0.));
#6364=DIRECTION('ref_axis',(1.,0.,0.));
#6365=DIRECTION('',(0.707106781186548,0.707106781186547,8.65956056235493E-17));
#6366=DIRECTION('center_axis',(0.,-1.,0.));
#6367=DIRECTION('ref_axis',(1.,0.,0.));
#6368=DIRECTION('center_axis',(0.,-1.,0.));
#6369=DIRECTION('ref_axis',(1.,0.,0.));
#6370=DIRECTION('',(0.,1.,0.));
#6371=DIRECTION('center_axis',(0.,1.,0.));
#6372=DIRECTION('ref_axis',(1.,0.,0.));
#6373=DIRECTION('center_axis',(0.,-1.,0.));
#6374=DIRECTION('ref_axis',(1.,0.,0.));
#6375=DIRECTION('',(-0.707106781186547,0.707106781186548,-8.65956056235493E-17));
#6376=DIRECTION('center_axis',(0.,-1.,0.));
#6377=DIRECTION('ref_axis',(0.,0.,-1.));
#6378=DIRECTION('center_axis',(0.,-1.,0.));
#6379=DIRECTION('ref_axis',(1.,0.,0.));
#6380=DIRECTION('center_axis',(0.,1.,0.));
#6381=DIRECTION('ref_axis',(1.,0.,0.));
#6382=DIRECTION('center_axis',(0.,1.,0.));
#6383=DIRECTION('ref_axis',(1.,0.,0.));
#6384=DIRECTION('',(-0.447213595499958,0.894427190999916,-5.47678698264203E-17));
#6385=DIRECTION('center_axis',(0.,-1.,0.));
#6386=DIRECTION('ref_axis',(1.,0.,0.));
#6387=DIRECTION('center_axis',(0.,1.,0.));
#6388=DIRECTION('ref_axis',(1.,0.,0.));
#6389=DIRECTION('',(0.,1.,0.));
#6390=DIRECTION('center_axis',(0.,1.,0.));
#6391=DIRECTION('ref_axis',(1.,0.,0.));
#6392=DIRECTION('center_axis',(0.,-1.,0.));
#6393=DIRECTION('ref_axis',(1.,0.,0.));
#6394=DIRECTION('',(-0.707106781186547,0.707106781186548,-8.65956056235493E-17));
#6395=DIRECTION('center_axis',(0.,-1.,0.));
#6396=DIRECTION('ref_axis',(0.,0.,-1.));
#6397=DIRECTION('center_axis',(0.866025403784439,0.,-0.5));
#6398=DIRECTION('ref_axis',(0.5,0.,0.866025403784439));
#6399=DIRECTION('',(-0.5,0.,-0.866025403784439));
#6400=DIRECTION('',(0.,-1.,0.));
#6401=DIRECTION('',(0.5,0.,0.866025403784439));
#6402=DIRECTION('',(0.,-1.,0.));
#6403=DIRECTION('center_axis',(1.20185167898973E-16,0.,-1.));
#6404=DIRECTION('ref_axis',(1.,0.,1.20185167898973E-16));
#6405=DIRECTION('',(-1.,0.,-1.20185167898973E-16));
#6406=DIRECTION('',(0.,-1.,0.));
#6407=DIRECTION('',(1.,0.,1.20185167898973E-16));
#6408=DIRECTION('center_axis',(-0.866025403784439,0.,-0.5));
#6409=DIRECTION('ref_axis',(0.5,0.,-0.866025403784439));
#6410=DIRECTION('',(-0.5,0.,0.866025403784439));
#6411=DIRECTION('',(0.,-1.,0.));
#6412=DIRECTION('',(0.5,0.,-0.866025403784439));
#6413=DIRECTION('center_axis',(-0.866025403784439,0.,0.5));
#6414=DIRECTION('ref_axis',(-0.5,0.,-0.866025403784439));
#6415=DIRECTION('',(0.5,0.,0.866025403784439));
#6416=DIRECTION('',(0.,-1.,0.));
#6417=DIRECTION('',(-0.5,0.,-0.866025403784439));
#6418=DIRECTION('center_axis',(-2.40370335797945E-16,0.,1.));
#6419=DIRECTION('ref_axis',(-1.,0.,-2.40370335797945E-16));
#6420=DIRECTION('',(1.,0.,2.40370335797945E-16));
#6421=DIRECTION('',(0.,-1.,0.));
#6422=DIRECTION('',(-1.,0.,-2.40370335797945E-16));
#6423=DIRECTION('center_axis',(0.866025403784439,0.,0.5));
#6424=DIRECTION('ref_axis',(-0.5,0.,0.866025403784439));
#6425=DIRECTION('',(0.5,0.,-0.866025403784439));
#6426=DIRECTION('',(-0.5,0.,0.866025403784439));
#6427=DIRECTION('center_axis',(0.,1.,0.));
#6428=DIRECTION('ref_axis',(1.,0.,0.));
#6429=DIRECTION('center_axis',(0.,-1.,0.));
#6430=DIRECTION('ref_axis',(0.,0.,-1.));
#6431=DIRECTION('',(0.,0.,1.));
#6432=DIRECTION('',(1.,0.,0.));
#6433=DIRECTION('',(0.,0.,1.));
#6434=DIRECTION('',(1.,0.,0.));
#6435=DIRECTION('',(0.,0.,1.));
#6436=DIRECTION('',(1.,0.,0.));
#6437=DIRECTION('',(0.,0.,1.));
#6438=DIRECTION('',(1.,0.,0.));
#6439=DIRECTION('',(0.,0.,1.));
#6440=DIRECTION('',(1.,0.,0.));
#6441=DIRECTION('',(0.,0.,1.));
#6442=DIRECTION('',(1.,0.,0.));
#6443=DIRECTION('',(0.,0.,1.));
#6444=DIRECTION('',(1.,0.,0.));
#6445=DIRECTION('',(8.65956056235493E-17,-8.65956056235493E-17,-1.));
#6446=DIRECTION('',(2.22044604925031E-16,1.,-8.65956056235494E-17));
#6447=DIRECTION('',(0.,-1.,2.22044604925031E-16));
#6448=DIRECTION('',(1.,0.,0.));
#6449=DIRECTION('',(8.65956056235493E-17,-8.65956056235493E-17,-1.));
#6450=DIRECTION('',(2.22044604925031E-16,1.,-8.65956056235494E-17));
#6451=DIRECTION('',(0.,-1.,2.22044604925031E-16));
#6452=DIRECTION('',(1.,0.,0.));
#6453=DIRECTION('',(0.,-1.,2.22044604925031E-16));
#6454=DIRECTION('',(1.,0.,0.));
#6455=DIRECTION('',(0.,-1.,2.22044604925031E-16));
#6456=DIRECTION('',(1.,0.,0.));
#6457=DIRECTION('',(0.,0.,1.));
#6458=DIRECTION('',(-1.,1.22464679914735E-16,0.));
#6459=DIRECTION('',(0.,0.,1.));
#6460=DIRECTION('',(1.,0.,0.));
#6461=DIRECTION('',(0.,0.,1.));
#6462=DIRECTION('',(1.,0.,0.));
#6463=DIRECTION('',(0.,0.,1.));
#6464=DIRECTION('',(1.,0.,0.));
#6465=CARTESIAN_POINT('',(0.,0.,0.));
#6466=CARTESIAN_POINT('',(0.,0.,0.));
#6467=CARTESIAN_POINT('',(0.,0.,0.));
#6468=CARTESIAN_POINT('Origin',(6.,-3.,-0.1));
#6469=CARTESIAN_POINT('',(5.67,-3.,0.));
#6470=CARTESIAN_POINT('Origin',(6.,-3.,0.));
#6471=CARTESIAN_POINT('',(5.67,-3.,1.2));
#6472=CARTESIAN_POINT('',(5.67,-3.,-0.1));
#6473=CARTESIAN_POINT('Origin',(6.,-3.,1.2));
#6474=CARTESIAN_POINT('Origin',(-6.,33.,-0.1));
#6475=CARTESIAN_POINT('',(-6.33,33.,0.));
#6476=CARTESIAN_POINT('Origin',(-6.,33.,0.));
#6477=CARTESIAN_POINT('',(-6.33,33.,1.2));
#6478=CARTESIAN_POINT('',(-6.33,33.,-0.1));
#6479=CARTESIAN_POINT('Origin',(-6.,33.,1.2));
#6480=CARTESIAN_POINT('Origin',(-6.,-3.,-0.1));
#6481=CARTESIAN_POINT('',(-6.33,-3.,0.));
#6482=CARTESIAN_POINT('Origin',(-6.,-3.,0.));
#6483=CARTESIAN_POINT('',(-6.33,-3.,1.2));
#6484=CARTESIAN_POINT('',(-6.33,-3.,-0.1));
#6485=CARTESIAN_POINT('Origin',(-6.,-3.,1.2));
#6486=CARTESIAN_POINT('Origin',(6.,33.,-0.1));
#6487=CARTESIAN_POINT('',(5.67,33.,0.));
#6488=CARTESIAN_POINT('Origin',(6.,33.,0.));
#6489=CARTESIAN_POINT('',(5.67,33.,1.2));
#6490=CARTESIAN_POINT('',(5.67,33.,-0.1));
#6491=CARTESIAN_POINT('Origin',(6.,33.,1.2));
#6492=CARTESIAN_POINT('Origin',(4.75,15.,-0.1));
#6493=CARTESIAN_POINT('',(4.41,15.,0.));
#6494=CARTESIAN_POINT('Origin',(4.75,15.,0.));
#6495=CARTESIAN_POINT('',(4.41,15.,1.2));
#6496=CARTESIAN_POINT('',(4.41,15.,-0.1));
#6497=CARTESIAN_POINT('Origin',(4.75,15.,1.2));
#6498=CARTESIAN_POINT('Origin',(-4.75,0.,-0.1));
#6499=CARTESIAN_POINT('',(-5.09,-4.163799117101E-17,0.));
#6500=CARTESIAN_POINT('Origin',(-4.75,0.,0.));
#6501=CARTESIAN_POINT('',(-5.09,4.163799117101E-17,1.2));
#6502=CARTESIAN_POINT('',(-5.09,-4.163799117101E-17,-0.1));
#6503=CARTESIAN_POINT('Origin',(-4.75,0.,1.2));
#6504=CARTESIAN_POINT('Origin',(-4.75,15.,-0.1));
#6505=CARTESIAN_POINT('',(-5.09,15.,0.));
#6506=CARTESIAN_POINT('Origin',(-4.75,15.,0.));
#6507=CARTESIAN_POINT('',(-5.09,15.,1.2));
#6508=CARTESIAN_POINT('',(-5.09,15.,-0.1));
#6509=CARTESIAN_POINT('Origin',(-4.75,15.,1.2));
#6510=CARTESIAN_POINT('Origin',(-4.75,30.,-0.1));
#6511=CARTESIAN_POINT('',(-5.09,30.,0.));
#6512=CARTESIAN_POINT('Origin',(-4.75,30.,0.));
#6513=CARTESIAN_POINT('',(-5.09,30.,1.2));
#6514=CARTESIAN_POINT('',(-5.09,30.,-0.1));
#6515=CARTESIAN_POINT('Origin',(-4.75,30.,1.2));
#6516=CARTESIAN_POINT('Origin',(4.75,0.,-0.1));
#6517=CARTESIAN_POINT('',(4.41,-4.163799117101E-17,0.));
#6518=CARTESIAN_POINT('Origin',(4.75,0.,0.));
#6519=CARTESIAN_POINT('',(4.41,4.163799117101E-17,1.2));
#6520=CARTESIAN_POINT('',(4.41,-4.163799117101E-17,-0.1));
#6521=CARTESIAN_POINT('Origin',(4.75,0.,1.2));
#6522=CARTESIAN_POINT('Origin',(4.75,30.,-0.1));
#6523=CARTESIAN_POINT('',(4.41,30.,0.));
#6524=CARTESIAN_POINT('Origin',(4.75,30.,0.));
#6525=CARTESIAN_POINT('',(4.41,30.,1.2));
#6526=CARTESIAN_POINT('',(4.41,30.,-0.1));
#6527=CARTESIAN_POINT('Origin',(4.75,30.,1.2));
#6528=CARTESIAN_POINT('Origin',(8.,34.,0.));
#6529=CARTESIAN_POINT('',(8.,34.,0.));
#6530=CARTESIAN_POINT('',(-8.,34.,0.));
#6531=CARTESIAN_POINT('',(8.,34.,0.));
#6532=CARTESIAN_POINT('',(-8.,34.,1.2));
#6533=CARTESIAN_POINT('',(-8.,34.,0.));
#6534=CARTESIAN_POINT('',(8.,34.,1.2));
#6535=CARTESIAN_POINT('',(8.,34.,1.2));
#6536=CARTESIAN_POINT('',(8.,34.,0.));
#6537=CARTESIAN_POINT('Origin',(8.,-4.,0.));
#6538=CARTESIAN_POINT('',(8.,-4.,0.));
#6539=CARTESIAN_POINT('',(8.,-4.,0.));
#6540=CARTESIAN_POINT('',(8.,-4.,1.2));
#6541=CARTESIAN_POINT('',(8.,-4.,1.2));
#6542=CARTESIAN_POINT('',(8.,-4.,0.));
#6543=CARTESIAN_POINT('Origin',(-8.,-4.,0.));
#6544=CARTESIAN_POINT('',(-8.,-4.,0.));
#6545=CARTESIAN_POINT('',(-8.,-4.,0.));
#6546=CARTESIAN_POINT('',(-8.,-4.,1.2));
#6547=CARTESIAN_POINT('',(-8.,-4.,1.2));
#6548=CARTESIAN_POINT('',(-8.,-4.,0.));
#6549=CARTESIAN_POINT('Origin',(-8.,34.,0.));
#6550=CARTESIAN_POINT('',(-8.,34.,0.));
#6551=CARTESIAN_POINT('',(-8.,34.,1.2));
#6552=CARTESIAN_POINT('Origin',(0.,15.,1.2));
#6553=CARTESIAN_POINT('Origin',(0.,15.,0.));
#6554=CARTESIAN_POINT('',(0.,0.,0.));
#6555=CARTESIAN_POINT('Origin',(-6.,-3.,-1.3));
#6556=CARTESIAN_POINT('',(-6.25,-3.,-1.3));
#6557=CARTESIAN_POINT('Origin',(-6.,-3.,-1.3));
#6558=CARTESIAN_POINT('',(-6.25,-3.,0.));
#6559=CARTESIAN_POINT('',(-6.25,-3.,-1.3));
#6560=CARTESIAN_POINT('Origin',(-6.,-3.,0.));
#6561=CARTESIAN_POINT('Origin',(-6.,-3.,-1.3));
#6562=CARTESIAN_POINT('Origin',(6.,-3.,-1.3));
#6563=CARTESIAN_POINT('',(5.75,-3.,-1.3));
#6564=CARTESIAN_POINT('Origin',(6.,-3.,-1.3));
#6565=CARTESIAN_POINT('',(5.75,-3.,0.));
#6566=CARTESIAN_POINT('',(5.75,-3.,-1.3));
#6567=CARTESIAN_POINT('Origin',(6.,-3.,0.));
#6568=CARTESIAN_POINT('Origin',(6.,-3.,-1.3));
#6569=CARTESIAN_POINT('Origin',(9.,-2.,-1.5));
#6570=CARTESIAN_POINT('',(9.,-2.,-1.5));
#6571=CARTESIAN_POINT('',(-9.,-2.,-1.5));
#6572=CARTESIAN_POINT('',(9.,-2.,-1.5));
#6573=CARTESIAN_POINT('',(-9.,-2.,0.));
#6574=CARTESIAN_POINT('',(-9.,-2.,-1.5));
#6575=CARTESIAN_POINT('',(9.,-2.,0.));
#6576=CARTESIAN_POINT('',(9.,-2.,0.));
#6577=CARTESIAN_POINT('',(9.,-2.,-1.5));
#6578=CARTESIAN_POINT('Origin',(9.,-4.,-1.5));
#6579=CARTESIAN_POINT('',(9.,-4.,-1.5));
#6580=CARTESIAN_POINT('',(9.,-4.,-1.5));
#6581=CARTESIAN_POINT('',(9.,-4.,0.));
#6582=CARTESIAN_POINT('',(9.,-4.,0.));
#6583=CARTESIAN_POINT('',(9.,-4.,-1.5));
#6584=CARTESIAN_POINT('Origin',(-9.,-4.,-1.5));
#6585=CARTESIAN_POINT('',(-9.,-4.,-1.5));
#6586=CARTESIAN_POINT('',(-9.,-4.,-1.5));
#6587=CARTESIAN_POINT('',(-9.,-4.,0.));
#6588=CARTESIAN_POINT('',(-9.,-4.,0.));
#6589=CARTESIAN_POINT('',(-9.,-4.,-1.5));
#6590=CARTESIAN_POINT('Origin',(-9.,-2.,-1.5));
#6591=CARTESIAN_POINT('',(-9.,-2.,-1.5));
#6592=CARTESIAN_POINT('',(-9.,-2.,0.));
#6593=CARTESIAN_POINT('Origin',(0.,-3.,0.));
#6594=CARTESIAN_POINT('Origin',(0.,-3.,-1.5));
#6595=CARTESIAN_POINT('',(0.,0.,0.));
#6596=CARTESIAN_POINT('Origin',(9.,-2.,-1.8));
#6597=CARTESIAN_POINT('',(9.,-2.,-1.8));
#6598=CARTESIAN_POINT('',(-9.,-2.,-1.8));
#6599=CARTESIAN_POINT('',(9.,-2.,-1.8));
#6600=CARTESIAN_POINT('',(-9.,-2.,-1.5));
#6601=CARTESIAN_POINT('',(-9.,-2.,-1.8));
#6602=CARTESIAN_POINT('',(9.,-2.,-1.5));
#6603=CARTESIAN_POINT('',(9.,-2.,-1.5));
#6604=CARTESIAN_POINT('',(9.,-2.,-1.8));
#6605=CARTESIAN_POINT('Origin',(9.,-4.,-1.8));
#6606=CARTESIAN_POINT('',(9.,-4.,-1.8));
#6607=CARTESIAN_POINT('',(9.,-4.,-1.8));
#6608=CARTESIAN_POINT('',(9.,-4.,-1.5));
#6609=CARTESIAN_POINT('',(9.,-4.,-1.5));
#6610=CARTESIAN_POINT('',(9.,-4.,-1.8));
#6611=CARTESIAN_POINT('Origin',(-9.,-4.,-1.8));
#6612=CARTESIAN_POINT('',(-9.,-4.,-1.8));
#6613=CARTESIAN_POINT('',(-9.,-4.,-1.8));
#6614=CARTESIAN_POINT('',(-9.,-4.,-1.5));
#6615=CARTESIAN_POINT('',(-9.,-4.,-1.5));
#6616=CARTESIAN_POINT('',(-9.,-4.,-1.8));
#6617=CARTESIAN_POINT('Origin',(-9.,-2.,-1.8));
#6618=CARTESIAN_POINT('',(-9.,-2.,-1.8));
#6619=CARTESIAN_POINT('',(-9.,-2.,-1.5));
#6620=CARTESIAN_POINT('Origin',(0.,-3.,-1.5));
#6621=CARTESIAN_POINT('Origin',(0.,-3.,-1.8));
#6622=CARTESIAN_POINT('',(0.,0.,0.));
#6623=CARTESIAN_POINT('Origin',(-6.,33.,-1.3));
#6624=CARTESIAN_POINT('',(-6.25,33.,-1.3));
#6625=CARTESIAN_POINT('Origin',(-6.,33.,-1.3));
#6626=CARTESIAN_POINT('',(-6.25,33.,0.));
#6627=CARTESIAN_POINT('',(-6.25,33.,-1.3));
#6628=CARTESIAN_POINT('Origin',(-6.,33.,0.));
#6629=CARTESIAN_POINT('Origin',(-6.,33.,-1.3));
#6630=CARTESIAN_POINT('Origin',(6.,33.,-1.3));
#6631=CARTESIAN_POINT('',(5.75,33.,-1.3));
#6632=CARTESIAN_POINT('Origin',(6.,33.,-1.3));
#6633=CARTESIAN_POINT('',(5.75,33.,0.));
#6634=CARTESIAN_POINT('',(5.75,33.,-1.3));
#6635=CARTESIAN_POINT('Origin',(6.,33.,0.));
#6636=CARTESIAN_POINT('Origin',(6.,33.,-1.3));
#6637=CARTESIAN_POINT('Origin',(9.,34.,-1.5));
#6638=CARTESIAN_POINT('',(9.,34.,-1.5));
#6639=CARTESIAN_POINT('',(-9.,34.,-1.5));
#6640=CARTESIAN_POINT('',(9.,34.,-1.5));
#6641=CARTESIAN_POINT('',(-9.,34.,0.));
#6642=CARTESIAN_POINT('',(-9.,34.,-1.5));
#6643=CARTESIAN_POINT('',(9.,34.,0.));
#6644=CARTESIAN_POINT('',(9.,34.,0.));
#6645=CARTESIAN_POINT('',(9.,34.,-1.5));
#6646=CARTESIAN_POINT('Origin',(9.,32.,-1.5));
#6647=CARTESIAN_POINT('',(9.,32.,-1.5));
#6648=CARTESIAN_POINT('',(9.,32.,-1.5));
#6649=CARTESIAN_POINT('',(9.,32.,0.));
#6650=CARTESIAN_POINT('',(9.,32.,0.));
#6651=CARTESIAN_POINT('',(9.,32.,-1.5));
#6652=CARTESIAN_POINT('Origin',(-9.,32.,-1.5));
#6653=CARTESIAN_POINT('',(-9.,32.,-1.5));
#6654=CARTESIAN_POINT('',(-9.,32.,-1.5));
#6655=CARTESIAN_POINT('',(-9.,32.,0.));
#6656=CARTESIAN_POINT('',(-9.,32.,0.));
#6657=CARTESIAN_POINT('',(-9.,32.,-1.5));
#6658=CARTESIAN_POINT('Origin',(-9.,34.,-1.5));
#6659=CARTESIAN_POINT('',(-9.,34.,-1.5));
#6660=CARTESIAN_POINT('',(-9.,34.,0.));
#6661=CARTESIAN_POINT('Origin',(0.,33.,0.));
#6662=CARTESIAN_POINT('Origin',(0.,33.,-1.5));
#6663=CARTESIAN_POINT('',(0.,0.,0.));
#6664=CARTESIAN_POINT('Origin',(9.,34.,-1.8));
#6665=CARTESIAN_POINT('',(9.,34.,-1.8));
#6666=CARTESIAN_POINT('',(-9.,34.,-1.8));
#6667=CARTESIAN_POINT('',(9.,34.,-1.8));
#6668=CARTESIAN_POINT('',(-9.,34.,-1.5));
#6669=CARTESIAN_POINT('',(-9.,34.,-1.8));
#6670=CARTESIAN_POINT('',(9.,34.,-1.5));
#6671=CARTESIAN_POINT('',(9.,34.,-1.5));
#6672=CARTESIAN_POINT('',(9.,34.,-1.8));
#6673=CARTESIAN_POINT('Origin',(9.,32.,-1.8));
#6674=CARTESIAN_POINT('',(9.,32.,-1.8));
#6675=CARTESIAN_POINT('',(9.,32.,-1.8));
#6676=CARTESIAN_POINT('',(9.,32.,-1.5));
#6677=CARTESIAN_POINT('',(9.,32.,-1.5));
#6678=CARTESIAN_POINT('',(9.,32.,-1.8));
#6679=CARTESIAN_POINT('Origin',(-9.,32.,-1.8));
#6680=CARTESIAN_POINT('',(-9.,32.,-1.8));
#6681=CARTESIAN_POINT('',(-9.,32.,-1.8));
#6682=CARTESIAN_POINT('',(-9.,32.,-1.5));
#6683=CARTESIAN_POINT('',(-9.,32.,-1.5));
#6684=CARTESIAN_POINT('',(-9.,32.,-1.8));
#6685=CARTESIAN_POINT('Origin',(-9.,34.,-1.8));
#6686=CARTESIAN_POINT('',(-9.,34.,-1.8));
#6687=CARTESIAN_POINT('',(-9.,34.,-1.5));
#6688=CARTESIAN_POINT('Origin',(0.,33.,-1.5));
#6689=CARTESIAN_POINT('Origin',(0.,33.,-1.8));
#6690=CARTESIAN_POINT('',(0.,0.,0.));
#6691=CARTESIAN_POINT('Origin',(-4.75,0.,1.2));
#6692=CARTESIAN_POINT('',(-5.175,-5.20474889637625E-17,2.4));
#6693=CARTESIAN_POINT('Origin',(-4.75,0.,2.4));
#6694=CARTESIAN_POINT('',(-5.175,-5.20474889637625E-17,1.2));
#6695=CARTESIAN_POINT('',(-5.175,-5.20474889637625E-17,1.2));
#6696=CARTESIAN_POINT('Origin',(-4.75,0.,1.2));
#6697=CARTESIAN_POINT('Origin',(-4.75,0.,1.2));
#6698=CARTESIAN_POINT('',(-5.395,-7.89897185450042E-17,2.4));
#6699=CARTESIAN_POINT('Origin',(-4.75,0.,2.4));
#6700=CARTESIAN_POINT('',(-5.395,-7.89897185450042E-17,1.2));
#6701=CARTESIAN_POINT('',(-5.395,-7.89897185450042E-17,1.2));
#6702=CARTESIAN_POINT('Origin',(-4.75,0.,1.2));
#6703=CARTESIAN_POINT('Origin',(-4.75,0.,2.4));
#6704=CARTESIAN_POINT('Origin',(-4.75,0.,1.2));
#6705=CARTESIAN_POINT('',(0.,0.,0.));
#6706=CARTESIAN_POINT('Origin',(4.75,0.,1.2));
#6707=CARTESIAN_POINT('',(4.325,-5.20474889637625E-17,2.4));
#6708=CARTESIAN_POINT('Origin',(4.75,0.,2.4));
#6709=CARTESIAN_POINT('',(4.325,-5.20474889637625E-17,1.2));
#6710=CARTESIAN_POINT('',(4.325,-5.20474889637625E-17,1.2));
#6711=CARTESIAN_POINT('Origin',(4.75,0.,1.2));
#6712=CARTESIAN_POINT('Origin',(4.75,0.,1.2));
#6713=CARTESIAN_POINT('',(4.105,-7.89897185450042E-17,2.4));
#6714=CARTESIAN_POINT('Origin',(4.75,0.,2.4));
#6715=CARTESIAN_POINT('',(4.105,-7.89897185450042E-17,1.2));
#6716=CARTESIAN_POINT('',(4.105,-7.89897185450042E-17,1.2));
#6717=CARTESIAN_POINT('Origin',(4.75,0.,1.2));
#6718=CARTESIAN_POINT('Origin',(4.75,0.,2.4));
#6719=CARTESIAN_POINT('Origin',(4.75,0.,1.2));
#6720=CARTESIAN_POINT('',(0.,0.,0.));
#6721=CARTESIAN_POINT('Origin',(-4.75,15.,1.2));
#6722=CARTESIAN_POINT('',(-5.175,15.,2.4));
#6723=CARTESIAN_POINT('Origin',(-4.75,15.,2.4));
#6724=CARTESIAN_POINT('',(-5.175,15.,1.2));
#6725=CARTESIAN_POINT('',(-5.175,15.,1.2));
#6726=CARTESIAN_POINT('Origin',(-4.75,15.,1.2));
#6727=CARTESIAN_POINT('Origin',(-4.75,15.,1.2));
#6728=CARTESIAN_POINT('',(-5.395,15.,2.4));
#6729=CARTESIAN_POINT('Origin',(-4.75,15.,2.4));
#6730=CARTESIAN_POINT('',(-5.395,15.,1.2));
#6731=CARTESIAN_POINT('',(-5.395,15.,1.2));
#6732=CARTESIAN_POINT('Origin',(-4.75,15.,1.2));
#6733=CARTESIAN_POINT('Origin',(-4.75,15.,2.4));
#6734=CARTESIAN_POINT('Origin',(-4.75,15.,1.2));
#6735=CARTESIAN_POINT('',(0.,0.,0.));
#6736=CARTESIAN_POINT('Origin',(4.75,15.,1.2));
#6737=CARTESIAN_POINT('',(4.325,15.,2.4));
#6738=CARTESIAN_POINT('Origin',(4.75,15.,2.4));
#6739=CARTESIAN_POINT('',(4.325,15.,1.2));
#6740=CARTESIAN_POINT('',(4.325,15.,1.2));
#6741=CARTESIAN_POINT('Origin',(4.75,15.,1.2));
#6742=CARTESIAN_POINT('Origin',(4.75,15.,1.2));
#6743=CARTESIAN_POINT('',(4.105,15.,2.4));
#6744=CARTESIAN_POINT('Origin',(4.75,15.,2.4));
#6745=CARTESIAN_POINT('',(4.105,15.,1.2));
#6746=CARTESIAN_POINT('',(4.105,15.,1.2));
#6747=CARTESIAN_POINT('Origin',(4.75,15.,1.2));
#6748=CARTESIAN_POINT('Origin',(4.75,15.,2.4));
#6749=CARTESIAN_POINT('Origin',(4.75,15.,1.2));
#6750=CARTESIAN_POINT('',(0.,0.,0.));
#6751=CARTESIAN_POINT('Origin',(-4.75,30.,1.2));
#6752=CARTESIAN_POINT('',(-5.175,30.,2.4));
#6753=CARTESIAN_POINT('Origin',(-4.75,30.,2.4));
#6754=CARTESIAN_POINT('',(-5.175,30.,1.2));
#6755=CARTESIAN_POINT('',(-5.175,30.,1.2));
#6756=CARTESIAN_POINT('Origin',(-4.75,30.,1.2));
#6757=CARTESIAN_POINT('Origin',(-4.75,30.,1.2));
#6758=CARTESIAN_POINT('',(-5.395,30.,2.4));
#6759=CARTESIAN_POINT('Origin',(-4.75,30.,2.4));
#6760=CARTESIAN_POINT('',(-5.395,30.,1.2));
#6761=CARTESIAN_POINT('',(-5.395,30.,1.2));
#6762=CARTESIAN_POINT('Origin',(-4.75,30.,1.2));
#6763=CARTESIAN_POINT('Origin',(-4.75,30.,2.4));
#6764=CARTESIAN_POINT('Origin',(-4.75,30.,1.2));
#6765=CARTESIAN_POINT('',(0.,0.,0.));
#6766=CARTESIAN_POINT('Origin',(4.75,30.,1.2));
#6767=CARTESIAN_POINT('',(4.325,30.,2.4));
#6768=CARTESIAN_POINT('Origin',(4.75,30.,2.4));
#6769=CARTESIAN_POINT('',(4.325,30.,1.2));
#6770=CARTESIAN_POINT('',(4.325,30.,1.2));
#6771=CARTESIAN_POINT('Origin',(4.75,30.,1.2));
#6772=CARTESIAN_POINT('Origin',(4.75,30.,1.2));
#6773=CARTESIAN_POINT('',(4.105,30.,2.4));
#6774=CARTESIAN_POINT('Origin',(4.75,30.,2.4));
#6775=CARTESIAN_POINT('',(4.105,30.,1.2));
#6776=CARTESIAN_POINT('',(4.105,30.,1.2));
#6777=CARTESIAN_POINT('Origin',(4.75,30.,1.2));
#6778=CARTESIAN_POINT('Origin',(4.75,30.,2.4));
#6779=CARTESIAN_POINT('Origin',(4.75,30.,1.2));
#6780=CARTESIAN_POINT('',(0.,0.,0.));
#6781=CARTESIAN_POINT('Origin',(0.,0.,0.));
#6782=CARTESIAN_POINT('',(-0.32,0.16,3.91886975727153E-17));
#6783=CARTESIAN_POINT('Origin',(0.,0.16,0.));
#6784=CARTESIAN_POINT('',(-0.32,0.,3.91886975727153E-17));
#6785=CARTESIAN_POINT('',(-0.32,0.,3.91886975727153E-17));
#6786=CARTESIAN_POINT('Origin',(0.,0.,0.));
#6787=CARTESIAN_POINT('Origin',(0.,0.,0.));
#6788=CARTESIAN_POINT('',(-0.6,0.16,7.34788079488412E-17));
#6789=CARTESIAN_POINT('Origin',(0.,0.16,0.));
#6790=CARTESIAN_POINT('',(-0.6,0.,7.34788079488412E-17));
#6791=CARTESIAN_POINT('',(-0.6,0.,7.34788079488412E-17));
#6792=CARTESIAN_POINT('Origin',(0.,0.,0.));
#6793=CARTESIAN_POINT('Origin',(0.,0.16,0.));
#6794=CARTESIAN_POINT('Origin',(0.,0.,0.));
#6795=CARTESIAN_POINT('',(0.,0.,0.));
#6796=CARTESIAN_POINT('Origin',(0.45,0.6,0.));
#6797=CARTESIAN_POINT('',(-0.45,0.6,-5.51091059616309E-17));
#6798=CARTESIAN_POINT('Origin',(0.,0.6,0.));
#6799=CARTESIAN_POINT('Origin',(0.,0.575,0.));
#6800=CARTESIAN_POINT('',(-0.5,0.55,-6.12323399573677E-17));
#6801=CARTESIAN_POINT('Origin',(0.,0.55,0.));
#6802=CARTESIAN_POINT('',(-0.475,0.575,-5.81707229594993E-17));
#6803=CARTESIAN_POINT('Origin',(0.,0.29,0.));
#6804=CARTESIAN_POINT('',(-0.5,0.0299999999999998,-6.12323399573677E-17));
#6805=CARTESIAN_POINT('Origin',(0.,0.0299999999999998,0.));
#6806=CARTESIAN_POINT('',(-0.5,0.29,-6.12323399573677E-17));
#6807=CARTESIAN_POINT('Origin',(0.,0.0150000000000001,0.));
#6808=CARTESIAN_POINT('',(-0.47,7.11236625150491E-17,-5.75583995599256E-17));
#6809=CARTESIAN_POINT('Origin',(0.,0.,0.));
#6810=CARTESIAN_POINT('',(-0.485,0.0150000000000001,-5.93953697586466E-17));
#6811=CARTESIAN_POINT('Origin',(0.32,0.,0.));
#6812=CARTESIAN_POINT('',(-0.32,-6.93889390390723E-18,-3.91886975727153E-17));
#6813=CARTESIAN_POINT('Origin',(0.,0.,0.));
#6814=CARTESIAN_POINT('Origin',(0.,-0.02,0.));
#6815=CARTESIAN_POINT('',(-0.2942,-0.0515999999999999,3.60291088309151E-17));
#6816=CARTESIAN_POINT('Origin',(0.,-0.0515999999999999,0.));
#6817=CARTESIAN_POINT('',(-0.31,-0.02,-3.7964050773568E-17));
#6818=CARTESIAN_POINT('Origin',(0.,-1.24,0.));
#6819=CARTESIAN_POINT('',(-0.2942,-2.4458,3.60291088309151E-17));
#6820=CARTESIAN_POINT('Origin',(0.,-2.4458,0.));
#6821=CARTESIAN_POINT('',(-0.2942,-1.24,-3.60291088309151E-17));
#6822=CARTESIAN_POINT('Origin',(0.,-2.47,0.));
#6823=CARTESIAN_POINT('',(-0.24,-2.5,-2.93915231795365E-17));
#6824=CARTESIAN_POINT('Origin',(0.,-2.5,0.));
#6825=CARTESIAN_POINT('',(-0.27,-2.47,-3.30654635769785E-17));
#6826=CARTESIAN_POINT('Origin',(0.,-2.5,0.));
#6827=CARTESIAN_POINT('Origin',(0.144337567297406,-0.6,-0.25));
#6828=CARTESIAN_POINT('',(0.288675134594813,-0.6,0.));
#6829=CARTESIAN_POINT('',(0.144337567297406,-0.6,-0.25));
#6830=CARTESIAN_POINT('',(0.288675134594813,-0.6,0.));
#6831=CARTESIAN_POINT('',(0.144337567297406,-0.96,-0.25));
#6832=CARTESIAN_POINT('',(0.144337567297406,-0.6,-0.25));
#6833=CARTESIAN_POINT('',(0.288675134594813,-0.96,0.));
#6834=CARTESIAN_POINT('',(0.288675134594813,-0.96,0.));
#6835=CARTESIAN_POINT('',(0.288675134594813,-0.6,0.));
#6836=CARTESIAN_POINT('Origin',(-0.144337567297406,-0.6,-0.25));
#6837=CARTESIAN_POINT('',(-0.144337567297406,-0.6,-0.25));
#6838=CARTESIAN_POINT('',(0.144337567297406,-0.6,-0.25));
#6839=CARTESIAN_POINT('',(-0.144337567297406,-0.96,-0.25));
#6840=CARTESIAN_POINT('',(-0.144337567297406,-0.6,-0.25));
#6841=CARTESIAN_POINT('',(0.144337567297406,-0.96,-0.25));
#6842=CARTESIAN_POINT('Origin',(-0.288675134594813,-0.6,-8.32667268468867E-17));
#6843=CARTESIAN_POINT('',(-0.288675134594813,-0.6,-3.53525079574969E-17));
#6844=CARTESIAN_POINT('',(-0.144337567297406,-0.6,-0.25));
#6845=CARTESIAN_POINT('',(-0.288675134594813,-0.96,-5.55111512312578E-17));
#6846=CARTESIAN_POINT('',(-0.288675134594813,-0.6,-3.53525079574969E-17));
#6847=CARTESIAN_POINT('',(-0.144337567297406,-0.96,-0.25));
#6848=CARTESIAN_POINT('Origin',(-0.144337567297407,-0.6,0.25));
#6849=CARTESIAN_POINT('',(-0.144337567297407,-0.6,0.25));
#6850=CARTESIAN_POINT('',(-0.288675134594813,-0.6,-3.53525079574969E-17));
#6851=CARTESIAN_POINT('',(-0.144337567297407,-0.96,0.25));
#6852=CARTESIAN_POINT('',(-0.144337567297407,-0.6,0.25));
#6853=CARTESIAN_POINT('',(-0.288675134594813,-0.96,-3.53525079574969E-17));
#6854=CARTESIAN_POINT('Origin',(0.144337567297406,-0.6,0.25));
#6855=CARTESIAN_POINT('',(0.144337567297406,-0.6,0.25));
#6856=CARTESIAN_POINT('',(-0.144337567297407,-0.6,0.25));
#6857=CARTESIAN_POINT('',(0.144337567297406,-0.96,0.25));
#6858=CARTESIAN_POINT('',(0.144337567297406,-0.6,0.25));
#6859=CARTESIAN_POINT('',(-0.144337567297407,-0.96,0.25));
#6860=CARTESIAN_POINT('Origin',(0.288675134594813,-0.6,0.));
#6861=CARTESIAN_POINT('',(0.144337567297406,-0.6,0.25));
#6862=CARTESIAN_POINT('',(0.144337567297406,-0.96,0.25));
#6863=CARTESIAN_POINT('Origin',(0.,-0.6,0.));
#6864=CARTESIAN_POINT('Origin',(0.,-0.96,0.));
#6865=CARTESIAN_POINT('',(0.,0.,0.));
#6866=CARTESIAN_POINT('',(0.,0.,0.));
#6867=CARTESIAN_POINT('Origin',(0.,0.,0.));
#6868=CARTESIAN_POINT('',(-2.05,-1.65,2.51052593825207E-16));
#6869=CARTESIAN_POINT('Origin',(0.,-1.65,0.));
#6870=CARTESIAN_POINT('',(-2.05,-1.14891252930761,-2.51052593825207E-16));
#6871=CARTESIAN_POINT('',(-2.05,0.,2.51052593825207E-16));
#6872=CARTESIAN_POINT('Origin',(0.,-1.14891252930761,0.));
#6873=CARTESIAN_POINT('Origin',(0.,0.,0.));
#6874=CARTESIAN_POINT('',(-2.05,1.14891252930761,2.51052593825207E-16));
#6875=CARTESIAN_POINT('Origin',(0.,1.14891252930761,0.));
#6876=CARTESIAN_POINT('',(-2.05,1.65,-2.51052593825207E-16));
#6877=CARTESIAN_POINT('',(-2.05,0.,2.51052593825207E-16));
#6878=CARTESIAN_POINT('Origin',(0.,1.65,0.));
#6879=CARTESIAN_POINT('Origin',(0.,0.,0.));
#6880=CARTESIAN_POINT('',(-1.43895998899814E-16,-1.76221774462768E-32,-2.35));
#6881=CARTESIAN_POINT('',(-1.43895998899814E-16,-1.76221774462768E-32,2.35));
#6882=CARTESIAN_POINT('Origin',(0.,0.,0.));
#6883=CARTESIAN_POINT('Origin',(0.,1.55,-1.49));
#6884=CARTESIAN_POINT('',(-3.76384615384615,1.55,-2.13));
#6885=CARTESIAN_POINT('',(-1.81744325908679,1.55,-2.13));
#6886=CARTESIAN_POINT('',(0.,1.55,-2.13));
#6887=CARTESIAN_POINT('',(-2.46585583768694,1.55,-1.32648218523477));
#6888=CARTESIAN_POINT('',(-1.68,1.55,-0.84));
#6889=CARTESIAN_POINT('Origin',(0.,1.55,0.));
#6890=CARTESIAN_POINT('Origin',(0.,1.55,-1.49));
#6891=CARTESIAN_POINT('',(1.81744325908679,1.55,-2.13));
#6892=CARTESIAN_POINT('',(3.76384615384615,1.55,-2.13));
#6893=CARTESIAN_POINT('',(0.,1.55,-2.13));
#6894=CARTESIAN_POINT('',(2.46585583768694,1.55,-1.32648218523477));
#6895=CARTESIAN_POINT('Origin',(0.,1.55,0.));
#6896=CARTESIAN_POINT('',(3.78,1.55,-2.14));
#6897=CARTESIAN_POINT('Origin',(0.,-1.55,-1.49));
#6898=CARTESIAN_POINT('',(-1.81744325908679,-1.55,-2.13));
#6899=CARTESIAN_POINT('',(-3.76384615384615,-1.55,-2.13));
#6900=CARTESIAN_POINT('',(0.,-1.55,-2.13));
#6901=CARTESIAN_POINT('',(-2.46585583768694,-1.55,-1.32648218523477));
#6902=CARTESIAN_POINT('Origin',(0.,-1.55,0.));
#6903=CARTESIAN_POINT('',(-1.68,-1.55,-0.84));
#6904=CARTESIAN_POINT('Origin',(-3.78,0.,-2.14));
#6905=CARTESIAN_POINT('',(-3.76384615384615,0.,-2.13));
#6906=CARTESIAN_POINT('',(-2.46585583768694,0.,-1.32648218523477));
#6907=CARTESIAN_POINT('Origin',(0.,-1.55,-1.49));
#6908=CARTESIAN_POINT('',(3.76384615384615,-1.55,-2.13));
#6909=CARTESIAN_POINT('',(1.81744325908679,-1.55,-2.13));
#6910=CARTESIAN_POINT('',(0.,-1.55,-2.13));
#6911=CARTESIAN_POINT('',(2.46585583768694,-1.55,-1.32648218523477));
#6912=CARTESIAN_POINT('',(3.78,-1.55,-2.14));
#6913=CARTESIAN_POINT('Origin',(0.,-1.55,0.));
#6914=CARTESIAN_POINT('Origin',(1.68,0.,-0.84));
#6915=CARTESIAN_POINT('',(3.76384615384615,0.,-2.13));
#6916=CARTESIAN_POINT('',(2.46585583768694,0.,-1.32648218523477));
#6917=CARTESIAN_POINT('Origin',(0.,0.,-2.13));
#6918=CARTESIAN_POINT('',(-6.35,1.9,-2.13));
#6919=CARTESIAN_POINT('',(-6.35,-1.9,-2.13));
#6920=CARTESIAN_POINT('',(-6.35,1.9,-2.13));
#6921=CARTESIAN_POINT('',(6.35,-1.9,-2.13));
#6922=CARTESIAN_POINT('',(-6.35,-1.9,-2.13));
#6923=CARTESIAN_POINT('',(6.35,1.9,-2.13));
#6924=CARTESIAN_POINT('',(6.35,-1.9,-2.13));
#6925=CARTESIAN_POINT('',(6.35,1.9,-2.13));
#6926=CARTESIAN_POINT('',(4.1,7.9602041944578E-17,-2.13));
#6927=CARTESIAN_POINT('Origin',(4.75,0.,-2.13));
#6928=CARTESIAN_POINT('',(-5.4,7.9602041944578E-17,-2.13));
#6929=CARTESIAN_POINT('Origin',(-4.75,0.,-2.13));
#6930=CARTESIAN_POINT('',(1.81744325908679,-1.65,-2.13));
#6931=CARTESIAN_POINT('',(1.81744325908679,0.,-2.13));
#6932=CARTESIAN_POINT('',(-1.81744325908679,-1.65,-2.13));
#6933=CARTESIAN_POINT('',(0.,-1.65,-2.13));
#6934=CARTESIAN_POINT('',(-1.81744325908679,0.,-2.13));
#6935=CARTESIAN_POINT('',(-1.81744325908679,1.65,-2.13));
#6936=CARTESIAN_POINT('',(-1.81744325908679,0.,-2.13));
#6937=CARTESIAN_POINT('',(1.81744325908679,1.65,-2.13));
#6938=CARTESIAN_POINT('',(0.,1.65,-2.13));
#6939=CARTESIAN_POINT('',(1.81744325908679,0.,-2.13));
#6940=CARTESIAN_POINT('Origin',(0.,0.,0.));
#6941=CARTESIAN_POINT('Origin',(0.,1.65,0.));
#6942=CARTESIAN_POINT('Origin',(0.,-1.65,0.));
#6943=CARTESIAN_POINT('Origin',(0.,-1.65,0.));
#6944=CARTESIAN_POINT('Origin',(0.,1.65,0.));
#6945=CARTESIAN_POINT('Origin',(3.35,1.4,-3.33));
#6946=CARTESIAN_POINT('',(3.35,1.4,-3.33));
#6947=CARTESIAN_POINT('',(-3.35,1.4,-3.33));
#6948=CARTESIAN_POINT('',(1.675,1.4,-3.33));
#6949=CARTESIAN_POINT('',(3.35,1.4,-2.83));
#6950=CARTESIAN_POINT('',(3.35,1.4,-3.33));
#6951=CARTESIAN_POINT('',(-3.35,1.4,-2.83));
#6952=CARTESIAN_POINT('',(3.35,1.4,-2.83));
#6953=CARTESIAN_POINT('',(-3.35,1.4,-3.33));
#6954=CARTESIAN_POINT('Origin',(3.35,-1.4,-3.33));
#6955=CARTESIAN_POINT('',(3.35,-1.4,-3.33));
#6956=CARTESIAN_POINT('',(3.35,-0.7,-3.33));
#6957=CARTESIAN_POINT('',(3.35,-1.4,-2.83));
#6958=CARTESIAN_POINT('',(3.35,-1.4,-3.33));
#6959=CARTESIAN_POINT('',(3.35,-1.4,-2.83));
#6960=CARTESIAN_POINT('Origin',(-3.35,-1.4,-3.33));
#6961=CARTESIAN_POINT('',(-3.35,-1.4,-3.33));
#6962=CARTESIAN_POINT('',(-1.675,-1.4,-3.33));
#6963=CARTESIAN_POINT('',(-3.35,-1.4,-2.83));
#6964=CARTESIAN_POINT('',(-3.35,-1.4,-3.33));
#6965=CARTESIAN_POINT('',(-3.35,-1.4,-2.83));
#6966=CARTESIAN_POINT('Origin',(-3.35,1.4,-3.33));
#6967=CARTESIAN_POINT('',(-3.35,0.7,-3.33));
#6968=CARTESIAN_POINT('',(-3.35,1.4,-2.83));
#6969=CARTESIAN_POINT('Origin',(0.,0.,-2.83));
#6970=CARTESIAN_POINT('Origin',(-4.75,0.,-3.33));
#6971=CARTESIAN_POINT('',(-5.4,-7.9602041944578E-17,-3.33));
#6972=CARTESIAN_POINT('Origin',(-4.75,0.,-3.33));
#6973=CARTESIAN_POINT('',(-5.4,-7.9602041944578E-17,-3.33));
#6974=CARTESIAN_POINT('Origin',(4.75,0.,-3.33));
#6975=CARTESIAN_POINT('',(4.1,-7.9602041944578E-17,-3.33));
#6976=CARTESIAN_POINT('Origin',(4.75,0.,-3.33));
#6977=CARTESIAN_POINT('',(4.1,-7.9602041944578E-17,-3.33));
#6978=CARTESIAN_POINT('Origin',(6.35,1.9,-3.33));
#6979=CARTESIAN_POINT('',(6.35,1.9,-3.33));
#6980=CARTESIAN_POINT('',(-6.35,1.9,-3.33));
#6981=CARTESIAN_POINT('',(6.35,1.9,-3.33));
#6982=CARTESIAN_POINT('',(-6.35,1.9,-3.33));
#6983=CARTESIAN_POINT('',(6.35,1.9,-3.33));
#6984=CARTESIAN_POINT('Origin',(6.35,-1.9,-3.33));
#6985=CARTESIAN_POINT('',(6.35,-1.9,-3.33));
#6986=CARTESIAN_POINT('',(6.35,-1.9,-3.33));
#6987=CARTESIAN_POINT('',(6.35,-1.9,-3.33));
#6988=CARTESIAN_POINT('Origin',(-6.35,-1.9,-3.33));
#6989=CARTESIAN_POINT('',(-6.35,-1.9,-3.33));
#6990=CARTESIAN_POINT('',(-6.35,-1.9,-3.33));
#6991=CARTESIAN_POINT('',(-6.35,-1.9,-3.33));
#6992=CARTESIAN_POINT('Origin',(-6.35,1.9,-3.33));
#6993=CARTESIAN_POINT('',(-6.35,1.9,-3.33));
#6994=CARTESIAN_POINT('Origin',(0.,0.,-3.33));
#6995=CARTESIAN_POINT('',(0.,0.,0.));
#6996=CARTESIAN_POINT('Origin',(0.,0.,0.));
#6997=CARTESIAN_POINT('',(-1.8,-0.85,-2.20436423846524E-16));
#6998=CARTESIAN_POINT('Origin',(0.,-0.85,0.));
#6999=CARTESIAN_POINT('',(-1.8,0.85,-2.20436423846524E-16));
#7000=CARTESIAN_POINT('',(-1.8,0.,-2.20436423846524E-16));
#7001=CARTESIAN_POINT('Origin',(0.,0.85,0.));
#7002=CARTESIAN_POINT('Origin',(2.19089023002066,0.85,0.));
#7003=CARTESIAN_POINT('',(2.19089023002066,0.85,0.));
#7004=CARTESIAN_POINT('Origin',(0.,0.85,0.));
#7005=CARTESIAN_POINT('Origin',(3.99680288865056E-15,0.,0.));
#7006=CARTESIAN_POINT('',(3.85290688975075E-15,-1.76221774462768E-32,2.35));
#7007=CARTESIAN_POINT('',(3.85290688975075E-15,-1.76221774462768E-32,-2.35));
#7008=CARTESIAN_POINT('Origin',(3.99680288865056E-15,0.,0.));
#7009=CARTESIAN_POINT('',(2.19089023002066,-0.85,0.));
#7010=CARTESIAN_POINT('Origin',(0.,-0.85,0.));
#7011=CARTESIAN_POINT('Origin',(1.8,-0.85,0.));
#7012=CARTESIAN_POINT('Origin',(0.,1.55,0.));
#7013=CARTESIAN_POINT('',(1.42894191624432,1.8,0.825000000000001));
#7014=CARTESIAN_POINT('',(1.53744468918255,1.55,0.598968970568896));
#7015=CARTESIAN_POINT('Ctrl Pts',(1.42894191624432,1.8,0.825000000000001));
#7016=CARTESIAN_POINT('Ctrl Pts',(1.44466308895875,1.8,0.797770130104052));
#7017=CARTESIAN_POINT('Ctrl Pts',(1.46055812562105,1.79370633789704,0.768258557763732));
#7018=CARTESIAN_POINT('Ctrl Pts',(1.48824888379079,1.76817777258318,0.713138492740816));
#7019=CARTESIAN_POINT('Ctrl Pts',(1.50008999307766,1.74894552961493,0.687551581002689));
#7020=CARTESIAN_POINT('Ctrl Pts',(1.51812136280714,1.70460745840382,0.646764802471699));
#7021=CARTESIAN_POINT('Ctrl Pts',(1.52552758004446,1.67652816181843,0.628833667319578));
#7022=CARTESIAN_POINT('Ctrl Pts',(1.53516661651472,1.61494799959182,0.604921184808251));
#7023=CARTESIAN_POINT('Ctrl Pts',(1.53744468918255,1.58144291640553,0.598968970568896));
#7024=CARTESIAN_POINT('Ctrl Pts',(1.53744468918255,1.55,0.598968970568896));
#7025=CARTESIAN_POINT('',(1.42894191624432,1.3,0.825000000000001));
#7026=CARTESIAN_POINT('Ctrl Pts',(1.42894191624432,1.3,0.825000000000001));
#7027=CARTESIAN_POINT('Ctrl Pts',(1.4132207435299,1.3,0.852229869895949));
#7028=CARTESIAN_POINT('Ctrl Pts',(1.39561049050871,1.30629366210296,0.880751161609749));
#7029=CARTESIAN_POINT('Ctrl Pts',(1.36172049302549,1.33182222741682,0.932292094146256));
#7030=CARTESIAN_POINT('Ctrl Pts',(1.34548213209931,1.35105447038507,0.955340251466734));
#7031=CARTESIAN_POINT('Ctrl Pts',(1.31917543061769,1.39539254159618,0.99134926498299));
#7032=CARTESIAN_POINT('Ctrl Pts',(1.30734972067592,1.42347183818157,1.00672880483252));
#7033=CARTESIAN_POINT('Ctrl Pts',(1.29146042158868,1.48505200040818,1.02703269653942));
#7034=CARTESIAN_POINT('Ctrl Pts',(1.28744468918255,1.51855708359447,1.03198167246111));
#7035=CARTESIAN_POINT('Ctrl Pts',(1.28744468918255,1.58144291640553,1.03198167246111));
#7036=CARTESIAN_POINT('Ctrl Pts',(1.29146042158868,1.61494799959182,1.02703269653942));
#7037=CARTESIAN_POINT('Ctrl Pts',(1.30734972067592,1.67652816181843,1.00672880483252));
#7038=CARTESIAN_POINT('Ctrl Pts',(1.31917543061769,1.70460745840382,0.991349264982991));
#7039=CARTESIAN_POINT('Ctrl Pts',(1.34548213209931,1.74894552961493,0.955340251466735));
#7040=CARTESIAN_POINT('Ctrl Pts',(1.36172049302549,1.76817777258318,0.932292094146256));
#7041=CARTESIAN_POINT('Ctrl Pts',(1.39561049050871,1.79370633789704,0.880751161609749));
#7042=CARTESIAN_POINT('Ctrl Pts',(1.4132207435299,1.8,0.85222986989595));
#7043=CARTESIAN_POINT('Ctrl Pts',(1.42894191624432,1.8,0.825000000000001));
#7044=CARTESIAN_POINT('Ctrl Pts',(1.53744468918255,1.55,0.598968970568896));
#7045=CARTESIAN_POINT('Ctrl Pts',(1.53744468918255,1.51855708359447,0.598968970568896));
#7046=CARTESIAN_POINT('Ctrl Pts',(1.53516661651472,1.48505200040818,0.60492118480825));
#7047=CARTESIAN_POINT('Ctrl Pts',(1.52552758004446,1.42347183818157,0.628833667319578));
#7048=CARTESIAN_POINT('Ctrl Pts',(1.51812136280714,1.39539254159618,0.646764802471699));
#7049=CARTESIAN_POINT('Ctrl Pts',(1.50008999307766,1.35105447038507,0.687551581002689));
#7050=CARTESIAN_POINT('Ctrl Pts',(1.48824888379079,1.33182222741682,0.713138492740816));
#7051=CARTESIAN_POINT('Ctrl Pts',(1.46055812562105,1.30629366210296,0.768258557763732));
#7052=CARTESIAN_POINT('Ctrl Pts',(1.44466308895875,1.3,0.797770130104052));
#7053=CARTESIAN_POINT('Ctrl Pts',(1.42894191624432,1.3,0.825000000000001));
#7054=CARTESIAN_POINT('',(0.963525491562421,1.55,0.267616567329818));
#7055=CARTESIAN_POINT('',(0.125,1.55,-0.21650635094611));
#7056=CARTESIAN_POINT('Ctrl Pts',(0.963525491562421,1.55,0.267616567329818));
#7057=CARTESIAN_POINT('Ctrl Pts',(0.963525491562421,1.5815373526696,0.267616567329818));
#7058=CARTESIAN_POINT('Ctrl Pts',(0.961833761492987,1.61508042700263,0.273949373987484));
#7059=CARTESIAN_POINT('Ctrl Pts',(0.954308486908894,1.67663267125761,0.299111603474268));
#7060=CARTESIAN_POINT('Ctrl Pts',(0.948394987258249,1.70465411363682,0.31788699900678));
#7061=CARTESIAN_POINT('Ctrl Pts',(0.933155485613026,1.74889618382539,0.360174810895352));
#7062=CARTESIAN_POINT('Ctrl Pts',(0.92278792026947,1.76811531482682,0.386546956384144));
#7063=CARTESIAN_POINT('Ctrl Pts',(0.897143218189782,1.79367084275751,0.442820664919227));
#7064=CARTESIAN_POINT('Ctrl Pts',(0.881791875377343,1.8,0.472691670144998));
#7065=CARTESIAN_POINT('Ctrl Pts',(0.850258932191534,1.8,0.527308329855003));
#7066=CARTESIAN_POINT('Ctrl Pts',(0.832065554235658,1.79367084275751,0.555538485325664));
#7067=CARTESIAN_POINT('Ctrl Pts',(0.796153444118959,1.76811531482682,0.605884303066698));
#7068=CARTESIAN_POINT('Ctrl Pts',(0.778498278845144,1.74889618382539,0.62804895077401));
#7069=CARTESIAN_POINT('Ctrl Pts',(0.749495710301794,1.70465411363682,0.662390652284073));
#7070=CARTESIAN_POINT('Ctrl Pts',(0.73619249062986,1.67663267125761,0.676899590973058));
#7071=CARTESIAN_POINT('Ctrl Pts',(0.718163997970498,1.61508042700263,0.695997784676728));
#7072=CARTESIAN_POINT('Ctrl Pts',(0.713525491562421,1.5815373526696,0.700629269222037));
#7073=CARTESIAN_POINT('Ctrl Pts',(0.713525491562421,1.5184626473304,0.700629269222037));
#7074=CARTESIAN_POINT('Ctrl Pts',(0.718163997970498,1.48491957299737,0.695997784676728));
#7075=CARTESIAN_POINT('Ctrl Pts',(0.73619249062986,1.42336732874239,0.676899590973058));
#7076=CARTESIAN_POINT('Ctrl Pts',(0.749495710301794,1.39534588636318,0.662390652284073));
#7077=CARTESIAN_POINT('Ctrl Pts',(0.778498278845144,1.35110381617461,0.62804895077401));
#7078=CARTESIAN_POINT('Ctrl Pts',(0.796153444118959,1.33188468517318,0.605884303066698));
#7079=CARTESIAN_POINT('Ctrl Pts',(0.832065554235658,1.30632915724249,0.555538485325664));
#7080=CARTESIAN_POINT('Ctrl Pts',(0.850258932191534,1.3,0.527308329855003));
#7081=CARTESIAN_POINT('Ctrl Pts',(0.881791875377343,1.3,0.472691670144998));
#7082=CARTESIAN_POINT('Ctrl Pts',(0.897143218189782,1.30632915724249,0.442820664919227));
#7083=CARTESIAN_POINT('Ctrl Pts',(0.92278792026947,1.33188468517318,0.386546956384144));
#7084=CARTESIAN_POINT('Ctrl Pts',(0.933155485613026,1.35110381617461,0.360174810895352));
#7085=CARTESIAN_POINT('Ctrl Pts',(0.948394987258249,1.39534588636318,0.31788699900678));
#7086=CARTESIAN_POINT('Ctrl Pts',(0.954308486908894,1.42336732874239,0.299111603474268));
#7087=CARTESIAN_POINT('Ctrl Pts',(0.961833761492987,1.48491957299738,0.273949373987484));
#7088=CARTESIAN_POINT('Ctrl Pts',(0.963525491562421,1.5184626473304,0.267616567329818));
#7089=CARTESIAN_POINT('Ctrl Pts',(0.963525491562421,1.55,0.267616567329818));
#7090=CARTESIAN_POINT('Origin',(0.,1.55,0.));
#7091=CARTESIAN_POINT('',(-0.713525491562421,1.55,-0.700629269222037));
#7092=CARTESIAN_POINT('Ctrl Pts',(-0.713525491562421,1.55,-0.700629269222037));
#7093=CARTESIAN_POINT('Ctrl Pts',(-0.713525491562421,1.5184626473304,-0.700629269222037));
#7094=CARTESIAN_POINT('Ctrl Pts',(-0.718163997970498,1.48491957299737,-0.695997784676728));
#7095=CARTESIAN_POINT('Ctrl Pts',(-0.73619249062986,1.42336732874239,-0.676899590973058));
#7096=CARTESIAN_POINT('Ctrl Pts',(-0.749495710301794,1.39534588636318,-0.662390652284073));
#7097=CARTESIAN_POINT('Ctrl Pts',(-0.778498278845144,1.35110381617461,-0.62804895077401));
#7098=CARTESIAN_POINT('Ctrl Pts',(-0.796153444118959,1.33188468517318,-0.605884303066698));
#7099=CARTESIAN_POINT('Ctrl Pts',(-0.832065554235658,1.30632915724249,-0.555538485325664));
#7100=CARTESIAN_POINT('Ctrl Pts',(-0.850258932191534,1.3,-0.527308329855003));
#7101=CARTESIAN_POINT('Ctrl Pts',(-0.881791875377343,1.3,-0.472691670144998));
#7102=CARTESIAN_POINT('Ctrl Pts',(-0.897143218189782,1.30632915724249,-0.442820664919227));
#7103=CARTESIAN_POINT('Ctrl Pts',(-0.92278792026947,1.33188468517318,-0.386546956384144));
#7104=CARTESIAN_POINT('Ctrl Pts',(-0.933155485613026,1.35110381617461,-0.360174810895352));
#7105=CARTESIAN_POINT('Ctrl Pts',(-0.948394987258249,1.39534588636318,-0.31788699900678));
#7106=CARTESIAN_POINT('Ctrl Pts',(-0.954308486908894,1.42336732874239,-0.299111603474268));
#7107=CARTESIAN_POINT('Ctrl Pts',(-0.961833761492986,1.48491957299737,-0.273949373987484));
#7108=CARTESIAN_POINT('Ctrl Pts',(-0.963525491562421,1.5184626473304,-0.267616567329818));
#7109=CARTESIAN_POINT('Ctrl Pts',(-0.963525491562421,1.5815373526696,-0.267616567329818));
#7110=CARTESIAN_POINT('Ctrl Pts',(-0.961833761492986,1.61508042700263,-0.273949373987484));
#7111=CARTESIAN_POINT('Ctrl Pts',(-0.954308486908894,1.67663267125761,-0.299111603474268));
#7112=CARTESIAN_POINT('Ctrl Pts',(-0.948394987258249,1.70465411363682,-0.31788699900678));
#7113=CARTESIAN_POINT('Ctrl Pts',(-0.933155485613026,1.74889618382539,-0.360174810895352));
#7114=CARTESIAN_POINT('Ctrl Pts',(-0.92278792026947,1.76811531482682,-0.386546956384144));
#7115=CARTESIAN_POINT('Ctrl Pts',(-0.897143218189782,1.79367084275751,-0.442820664919227));
#7116=CARTESIAN_POINT('Ctrl Pts',(-0.881791875377343,1.8,-0.472691670144998));
#7117=CARTESIAN_POINT('Ctrl Pts',(-0.850258932191534,1.8,-0.527308329855003));
#7118=CARTESIAN_POINT('Ctrl Pts',(-0.832065554235658,1.79367084275751,-0.555538485325664));
#7119=CARTESIAN_POINT('Ctrl Pts',(-0.796153444118959,1.76811531482682,-0.605884303066698));
#7120=CARTESIAN_POINT('Ctrl Pts',(-0.778498278845144,1.74889618382539,-0.62804895077401));
#7121=CARTESIAN_POINT('Ctrl Pts',(-0.749495710301794,1.70465411363682,-0.662390652284073));
#7122=CARTESIAN_POINT('Ctrl Pts',(-0.73619249062986,1.67663267125761,-0.676899590973058));
#7123=CARTESIAN_POINT('Ctrl Pts',(-0.718163997970498,1.61508042700263,-0.695997784676728));
#7124=CARTESIAN_POINT('Ctrl Pts',(-0.713525491562421,1.5815373526696,-0.700629269222037));
#7125=CARTESIAN_POINT('Ctrl Pts',(-0.713525491562421,1.55,-0.700629269222037));
#7126=CARTESIAN_POINT('',(-1.28744468918255,1.55,-1.03198167246111));
#7127=CARTESIAN_POINT('',(0.125,1.55,-0.21650635094611));
#7128=CARTESIAN_POINT('',(-1.42894191624432,1.3,-0.825000000000001));
#7129=CARTESIAN_POINT('Ctrl Pts',(-1.42894191624432,1.3,-0.825000000000001));
#7130=CARTESIAN_POINT('Ctrl Pts',(-1.4132207435299,1.3,-0.852229869895949));
#7131=CARTESIAN_POINT('Ctrl Pts',(-1.39561049050871,1.30629366210296,-0.880751161609749));
#7132=CARTESIAN_POINT('Ctrl Pts',(-1.36172049302549,1.33182222741682,-0.932292094146256));
#7133=CARTESIAN_POINT('Ctrl Pts',(-1.34548213209931,1.35105447038507,-0.955340251466735));
#7134=CARTESIAN_POINT('Ctrl Pts',(-1.31917543061769,1.39539254159618,-0.991349264982991));
#7135=CARTESIAN_POINT('Ctrl Pts',(-1.30734972067592,1.42347183818157,-1.00672880483252));
#7136=CARTESIAN_POINT('Ctrl Pts',(-1.29146042158868,1.48505200040818,-1.02703269653942));
#7137=CARTESIAN_POINT('Ctrl Pts',(-1.28744468918255,1.51855708359447,-1.03198167246111));
#7138=CARTESIAN_POINT('Ctrl Pts',(-1.28744468918255,1.55,-1.03198167246111));
#7139=CARTESIAN_POINT('',(-1.42894191624432,1.8,-0.825000000000001));
#7140=CARTESIAN_POINT('Ctrl Pts',(-1.42894191624432,1.8,-0.825000000000001));
#7141=CARTESIAN_POINT('Ctrl Pts',(-1.44466308895875,1.8,-0.797770130104052));
#7142=CARTESIAN_POINT('Ctrl Pts',(-1.46055812562105,1.79370633789704,-0.768258557763732));
#7143=CARTESIAN_POINT('Ctrl Pts',(-1.48824888379079,1.76817777258318,-0.713138492740816));
#7144=CARTESIAN_POINT('Ctrl Pts',(-1.50008999307766,1.74894552961493,-0.687551581002689));
#7145=CARTESIAN_POINT('Ctrl Pts',(-1.51812136280714,1.70460745840382,-0.646764802471699));
#7146=CARTESIAN_POINT('Ctrl Pts',(-1.52552758004446,1.67652816181843,-0.628833667319578));
#7147=CARTESIAN_POINT('Ctrl Pts',(-1.53516661651472,1.61494799959182,-0.60492118480825));
#7148=CARTESIAN_POINT('Ctrl Pts',(-1.53744468918255,1.58144291640553,-0.598968970568896));
#7149=CARTESIAN_POINT('Ctrl Pts',(-1.53744468918255,1.51855708359447,-0.598968970568896));
#7150=CARTESIAN_POINT('Ctrl Pts',(-1.53516661651472,1.48505200040818,-0.60492118480825));
#7151=CARTESIAN_POINT('Ctrl Pts',(-1.52552758004446,1.42347183818157,-0.628833667319578));
#7152=CARTESIAN_POINT('Ctrl Pts',(-1.51812136280714,1.39539254159618,-0.646764802471699));
#7153=CARTESIAN_POINT('Ctrl Pts',(-1.50008999307766,1.35105447038507,-0.687551581002689));
#7154=CARTESIAN_POINT('Ctrl Pts',(-1.48824888379079,1.33182222741682,-0.713138492740816));
#7155=CARTESIAN_POINT('Ctrl Pts',(-1.46055812562105,1.30629366210296,-0.768258557763732));
#7156=CARTESIAN_POINT('Ctrl Pts',(-1.44466308895875,1.3,-0.797770130104052));
#7157=CARTESIAN_POINT('Ctrl Pts',(-1.42894191624432,1.3,-0.825000000000001));
#7158=CARTESIAN_POINT('Ctrl Pts',(-1.28744468918255,1.55,-1.03198167246111));
#7159=CARTESIAN_POINT('Ctrl Pts',(-1.28744468918255,1.58144291640553,-1.03198167246111));
#7160=CARTESIAN_POINT('Ctrl Pts',(-1.29146042158868,1.61494799959182,-1.02703269653942));
#7161=CARTESIAN_POINT('Ctrl Pts',(-1.30734972067592,1.67652816181843,-1.00672880483252));
#7162=CARTESIAN_POINT('Ctrl Pts',(-1.31917543061769,1.70460745840382,-0.991349264982991));
#7163=CARTESIAN_POINT('Ctrl Pts',(-1.34548213209931,1.74894552961493,-0.955340251466734));
#7164=CARTESIAN_POINT('Ctrl Pts',(-1.36172049302549,1.76817777258318,-0.932292094146256));
#7165=CARTESIAN_POINT('Ctrl Pts',(-1.39561049050871,1.79370633789704,-0.880751161609749));
#7166=CARTESIAN_POINT('Ctrl Pts',(-1.4132207435299,1.8,-0.852229869895949));
#7167=CARTESIAN_POINT('Ctrl Pts',(-1.42894191624432,1.8,-0.825000000000001));
#7168=CARTESIAN_POINT('Origin',(0.,1.55,0.));
#7169=CARTESIAN_POINT('',(-1.65,0.85,-2.02066721859313E-16));
#7170=CARTESIAN_POINT('Origin',(0.,0.85,0.));
#7171=CARTESIAN_POINT('',(-1.65,2.25,-2.02066721859313E-16));
#7172=CARTESIAN_POINT('',(-1.65,1.55,-2.02066721859313E-16));
#7173=CARTESIAN_POINT('Origin',(0.,2.25,0.));
#7174=CARTESIAN_POINT('',(-1.42894191624432,1.3,0.825));
#7175=CARTESIAN_POINT('',(-1.42894191624432,1.8,0.825));
#7176=CARTESIAN_POINT('Ctrl Pts',(-1.42894191624432,1.3,0.825));
#7177=CARTESIAN_POINT('Ctrl Pts',(-1.44466308895875,1.3,0.797770130104051));
#7178=CARTESIAN_POINT('Ctrl Pts',(-1.46055812562105,1.30629366210296,0.768258557763731));
#7179=CARTESIAN_POINT('Ctrl Pts',(-1.48824888379079,1.33182222741682,0.713138492740815));
#7180=CARTESIAN_POINT('Ctrl Pts',(-1.50008999307766,1.35105447038507,0.687551581002688));
#7181=CARTESIAN_POINT('Ctrl Pts',(-1.51812136280714,1.39539254159618,0.646764802471698));
#7182=CARTESIAN_POINT('Ctrl Pts',(-1.52552758004446,1.42347183818157,0.628833667319577));
#7183=CARTESIAN_POINT('Ctrl Pts',(-1.53516661651472,1.48505200040818,0.604921184808249));
#7184=CARTESIAN_POINT('Ctrl Pts',(-1.53744468918255,1.51855708359447,0.598968970568895));
#7185=CARTESIAN_POINT('Ctrl Pts',(-1.53744468918255,1.58144291640553,0.598968970568895));
#7186=CARTESIAN_POINT('Ctrl Pts',(-1.53516661651472,1.61494799959182,0.604921184808249));
#7187=CARTESIAN_POINT('Ctrl Pts',(-1.52552758004446,1.67652816181843,0.628833667319577));
#7188=CARTESIAN_POINT('Ctrl Pts',(-1.51812136280714,1.70460745840382,0.646764802471698));
#7189=CARTESIAN_POINT('Ctrl Pts',(-1.50008999307766,1.74894552961493,0.687551581002688));
#7190=CARTESIAN_POINT('Ctrl Pts',(-1.48824888379079,1.76817777258318,0.713138492740815));
#7191=CARTESIAN_POINT('Ctrl Pts',(-1.46055812562105,1.79370633789704,0.768258557763731));
#7192=CARTESIAN_POINT('Ctrl Pts',(-1.44466308895875,1.8,0.797770130104051));
#7193=CARTESIAN_POINT('Ctrl Pts',(-1.42894191624432,1.8,0.825));
#7194=CARTESIAN_POINT('',(-1.28744468918255,1.55,1.03198167246111));
#7195=CARTESIAN_POINT('Ctrl Pts',(-1.42894191624432,1.8,0.825));
#7196=CARTESIAN_POINT('Ctrl Pts',(-1.4132207435299,1.8,0.852229869895948));
#7197=CARTESIAN_POINT('Ctrl Pts',(-1.39561049050871,1.79370633789704,0.880751161609747));
#7198=CARTESIAN_POINT('Ctrl Pts',(-1.36172049302549,1.76817777258318,0.932292094146255));
#7199=CARTESIAN_POINT('Ctrl Pts',(-1.34548213209931,1.74894552961493,0.955340251466733));
#7200=CARTESIAN_POINT('Ctrl Pts',(-1.31917543061769,1.70460745840382,0.991349264982989));
#7201=CARTESIAN_POINT('Ctrl Pts',(-1.30734972067592,1.67652816181843,1.00672880483252));
#7202=CARTESIAN_POINT('Ctrl Pts',(-1.29146042158868,1.61494799959182,1.02703269653942));
#7203=CARTESIAN_POINT('Ctrl Pts',(-1.28744468918255,1.58144291640553,1.03198167246111));
#7204=CARTESIAN_POINT('Ctrl Pts',(-1.28744468918255,1.55,1.03198167246111));
#7205=CARTESIAN_POINT('Ctrl Pts',(-1.28744468918255,1.55,1.03198167246111));
#7206=CARTESIAN_POINT('Ctrl Pts',(-1.28744468918255,1.51855708359447,1.03198167246111));
#7207=CARTESIAN_POINT('Ctrl Pts',(-1.29146042158868,1.48505200040818,1.02703269653942));
#7208=CARTESIAN_POINT('Ctrl Pts',(-1.30734972067592,1.42347183818157,1.00672880483252));
#7209=CARTESIAN_POINT('Ctrl Pts',(-1.31917543061769,1.39539254159618,0.99134926498299));
#7210=CARTESIAN_POINT('Ctrl Pts',(-1.34548213209931,1.35105447038508,0.955340251466733));
#7211=CARTESIAN_POINT('Ctrl Pts',(-1.36172049302549,1.33182222741682,0.932292094146255));
#7212=CARTESIAN_POINT('Ctrl Pts',(-1.39561049050871,1.30629366210296,0.880751161609748));
#7213=CARTESIAN_POINT('Ctrl Pts',(-1.4132207435299,1.3,0.852229869895949));
#7214=CARTESIAN_POINT('Ctrl Pts',(-1.42894191624432,1.3,0.825));
#7215=CARTESIAN_POINT('',(1.42894191624432,1.8,-0.825));
#7216=CARTESIAN_POINT('',(1.42894191624432,1.3,-0.825));
#7217=CARTESIAN_POINT('Ctrl Pts',(1.42894191624432,1.8,-0.825));
#7218=CARTESIAN_POINT('Ctrl Pts',(1.4132207435299,1.8,-0.852229869895949));
#7219=CARTESIAN_POINT('Ctrl Pts',(1.39561049050871,1.79370633789704,-0.880751161609748));
#7220=CARTESIAN_POINT('Ctrl Pts',(1.36172049302549,1.76817777258318,-0.932292094146255));
#7221=CARTESIAN_POINT('Ctrl Pts',(1.34548213209931,1.74894552961493,-0.955340251466734));
#7222=CARTESIAN_POINT('Ctrl Pts',(1.31917543061769,1.70460745840382,-0.99134926498299));
#7223=CARTESIAN_POINT('Ctrl Pts',(1.30734972067592,1.67652816181843,-1.00672880483252));
#7224=CARTESIAN_POINT('Ctrl Pts',(1.29146042158868,1.61494799959182,-1.02703269653942));
#7225=CARTESIAN_POINT('Ctrl Pts',(1.28744468918255,1.58144291640553,-1.03198167246111));
#7226=CARTESIAN_POINT('Ctrl Pts',(1.28744468918255,1.51855708359447,-1.03198167246111));
#7227=CARTESIAN_POINT('Ctrl Pts',(1.29146042158868,1.48505200040818,-1.02703269653942));
#7228=CARTESIAN_POINT('Ctrl Pts',(1.30734972067592,1.42347183818157,-1.00672880483252));
#7229=CARTESIAN_POINT('Ctrl Pts',(1.31917543061769,1.39539254159618,-0.99134926498299));
#7230=CARTESIAN_POINT('Ctrl Pts',(1.34548213209931,1.35105447038507,-0.955340251466734));
#7231=CARTESIAN_POINT('Ctrl Pts',(1.36172049302549,1.33182222741682,-0.932292094146255));
#7232=CARTESIAN_POINT('Ctrl Pts',(1.39561049050871,1.30629366210296,-0.880751161609748));
#7233=CARTESIAN_POINT('Ctrl Pts',(1.4132207435299,1.3,-0.852229869895948));
#7234=CARTESIAN_POINT('Ctrl Pts',(1.42894191624432,1.3,-0.825));
#7235=CARTESIAN_POINT('',(1.53744468918255,1.55,-0.598968970568895));
#7236=CARTESIAN_POINT('Ctrl Pts',(1.42894191624432,1.3,-0.825));
#7237=CARTESIAN_POINT('Ctrl Pts',(1.44466308895875,1.3,-0.797770130104051));
#7238=CARTESIAN_POINT('Ctrl Pts',(1.46055812562105,1.30629366210296,-0.768258557763731));
#7239=CARTESIAN_POINT('Ctrl Pts',(1.48824888379079,1.33182222741682,-0.713138492740815));
#7240=CARTESIAN_POINT('Ctrl Pts',(1.50008999307766,1.35105447038507,-0.687551581002688));
#7241=CARTESIAN_POINT('Ctrl Pts',(1.51812136280714,1.39539254159618,-0.646764802471698));
#7242=CARTESIAN_POINT('Ctrl Pts',(1.52552758004446,1.42347183818157,-0.628833667319577));
#7243=CARTESIAN_POINT('Ctrl Pts',(1.53516661651472,1.48505200040818,-0.604921184808249));
#7244=CARTESIAN_POINT('Ctrl Pts',(1.53744468918255,1.51855708359447,-0.598968970568895));
#7245=CARTESIAN_POINT('Ctrl Pts',(1.53744468918255,1.55,-0.598968970568895));
#7246=CARTESIAN_POINT('Ctrl Pts',(1.53744468918255,1.55,-0.598968970568895));
#7247=CARTESIAN_POINT('Ctrl Pts',(1.53744468918255,1.58144291640553,-0.598968970568895));
#7248=CARTESIAN_POINT('Ctrl Pts',(1.53516661651472,1.61494799959182,-0.604921184808249));
#7249=CARTESIAN_POINT('Ctrl Pts',(1.52552758004446,1.67652816181843,-0.628833667319577));
#7250=CARTESIAN_POINT('Ctrl Pts',(1.51812136280714,1.70460745840382,-0.646764802471698));
#7251=CARTESIAN_POINT('Ctrl Pts',(1.50008999307766,1.74894552961493,-0.687551581002688));
#7252=CARTESIAN_POINT('Ctrl Pts',(1.48824888379079,1.76817777258318,-0.713138492740815));
#7253=CARTESIAN_POINT('Ctrl Pts',(1.46055812562105,1.79370633789704,-0.768258557763731));
#7254=CARTESIAN_POINT('Ctrl Pts',(1.44466308895875,1.8,-0.797770130104051));
#7255=CARTESIAN_POINT('Ctrl Pts',(1.42894191624432,1.8,-0.825));
#7256=CARTESIAN_POINT('',(0.,1.3,-1.65));
#7257=CARTESIAN_POINT('',(0.,1.8,-1.65));
#7258=CARTESIAN_POINT('Ctrl Pts',(1.38777878078145E-17,1.3,-1.65));
#7259=CARTESIAN_POINT('Ctrl Pts',(0.0314423454288489,1.3,-1.65));
#7260=CARTESIAN_POINT('Ctrl Pts',(0.0649476351123396,1.30629366210296,-1.64900971937348));
#7261=CARTESIAN_POINT('Ctrl Pts',(0.126528390765307,1.33182222741682,-1.64543058688707));
#7262=CARTESIAN_POINT('Ctrl Pts',(0.154607860978348,1.35105447038507,-1.64289183246942));
#7263=CARTESIAN_POINT('Ctrl Pts',(0.198945932189457,1.39539254159618,-1.63811406745469));
#7264=CARTESIAN_POINT('Ctrl Pts',(0.218177859368546,1.42347183818157,-1.63556247215209));
#7265=CARTESIAN_POINT('Ctrl Pts',(0.243706194926033,1.48505200040818,-1.63195388134767));
#7266=CARTESIAN_POINT('Ctrl Pts',(0.25,1.51855708359447,-1.63095064303001));
#7267=CARTESIAN_POINT('Ctrl Pts',(0.25,1.58144291640553,-1.63095064303001));
#7268=CARTESIAN_POINT('Ctrl Pts',(0.243706194926033,1.61494799959182,-1.63195388134767));
#7269=CARTESIAN_POINT('Ctrl Pts',(0.218177859368546,1.67652816181843,-1.63556247215209));
#7270=CARTESIAN_POINT('Ctrl Pts',(0.198945932189457,1.70460745840382,-1.63811406745469));
#7271=CARTESIAN_POINT('Ctrl Pts',(0.154607860978349,1.74894552961493,-1.64289183246942));
#7272=CARTESIAN_POINT('Ctrl Pts',(0.126528390765307,1.76817777258318,-1.64543058688707));
#7273=CARTESIAN_POINT('Ctrl Pts',(0.0649476351123398,1.79370633789704,-1.64900971937348));
#7274=CARTESIAN_POINT('Ctrl Pts',(0.031442345428849,1.8,-1.65));
#7275=CARTESIAN_POINT('Ctrl Pts',(7.63278329429795E-17,1.8,-1.65));
#7276=CARTESIAN_POINT('',(-0.25,1.55,-1.63095064303001));
#7277=CARTESIAN_POINT('Ctrl Pts',(9.0205620750794E-17,1.8,-1.65));
#7278=CARTESIAN_POINT('Ctrl Pts',(-0.0314423454288488,1.8,-1.65));
#7279=CARTESIAN_POINT('Ctrl Pts',(-0.0649476351123396,1.79370633789704,
-1.64900971937348));
#7280=CARTESIAN_POINT('Ctrl Pts',(-0.126528390765307,1.76817777258318,-1.64543058688707));
#7281=CARTESIAN_POINT('Ctrl Pts',(-0.154607860978348,1.74894552961493,-1.64289183246942));
#7282=CARTESIAN_POINT('Ctrl Pts',(-0.198945932189456,1.70460745840382,-1.63811406745469));
#7283=CARTESIAN_POINT('Ctrl Pts',(-0.218177859368546,1.67652816181843,-1.63556247215209));
#7284=CARTESIAN_POINT('Ctrl Pts',(-0.243706194926033,1.61494799959182,-1.63195388134767));
#7285=CARTESIAN_POINT('Ctrl Pts',(-0.25,1.58144291640553,-1.63095064303001));
#7286=CARTESIAN_POINT('Ctrl Pts',(-0.25,1.55,-1.63095064303001));
#7287=CARTESIAN_POINT('Ctrl Pts',(-0.25,1.55,-1.63095064303001));
#7288=CARTESIAN_POINT('Ctrl Pts',(-0.25,1.51855708359447,-1.63095064303001));
#7289=CARTESIAN_POINT('Ctrl Pts',(-0.243706194926033,1.48505200040818,-1.63195388134767));
#7290=CARTESIAN_POINT('Ctrl Pts',(-0.218177859368546,1.42347183818157,-1.63556247215209));
#7291=CARTESIAN_POINT('Ctrl Pts',(-0.198945932189457,1.39539254159618,-1.63811406745469));
#7292=CARTESIAN_POINT('Ctrl Pts',(-0.154607860978349,1.35105447038507,-1.64289183246942));
#7293=CARTESIAN_POINT('Ctrl Pts',(-0.126528390765307,1.33182222741682,-1.64543058688707));
#7294=CARTESIAN_POINT('Ctrl Pts',(-0.0649476351123398,1.30629366210296,
-1.64900971937348));
#7295=CARTESIAN_POINT('Ctrl Pts',(-0.031442345428849,1.3,-1.65));
#7296=CARTESIAN_POINT('Ctrl Pts',(-4.85722573273506E-17,1.3,-1.65));
#7297=CARTESIAN_POINT('',(0.,1.8,1.65));
#7298=CARTESIAN_POINT('',(0.,1.3,1.65));
#7299=CARTESIAN_POINT('Ctrl Pts',(8.32667268468867E-17,1.8,1.65));
#7300=CARTESIAN_POINT('Ctrl Pts',(0.031442345428849,1.8,1.65));
#7301=CARTESIAN_POINT('Ctrl Pts',(0.0649476351123398,1.79370633789704,1.64900971937348));
#7302=CARTESIAN_POINT('Ctrl Pts',(0.126528390765307,1.76817777258318,1.64543058688707));
#7303=CARTESIAN_POINT('Ctrl Pts',(0.154607860978349,1.74894552961493,1.64289183246942));
#7304=CARTESIAN_POINT('Ctrl Pts',(0.198945932189457,1.70460745840382,1.63811406745469));
#7305=CARTESIAN_POINT('Ctrl Pts',(0.218177859368546,1.67652816181843,1.63556247215209));
#7306=CARTESIAN_POINT('Ctrl Pts',(0.243706194926033,1.61494799959182,1.63195388134767));
#7307=CARTESIAN_POINT('Ctrl Pts',(0.25,1.58144291640553,1.63095064303001));
#7308=CARTESIAN_POINT('Ctrl Pts',(0.25,1.51855708359447,1.63095064303001));
#7309=CARTESIAN_POINT('Ctrl Pts',(0.243706194926033,1.48505200040818,1.63195388134767));
#7310=CARTESIAN_POINT('Ctrl Pts',(0.218177859368546,1.42347183818157,1.63556247215209));
#7311=CARTESIAN_POINT('Ctrl Pts',(0.198945932189457,1.39539254159618,1.63811406745469));
#7312=CARTESIAN_POINT('Ctrl Pts',(0.154607860978348,1.35105447038507,1.64289183246942));
#7313=CARTESIAN_POINT('Ctrl Pts',(0.126528390765307,1.33182222741682,1.64543058688707));
#7314=CARTESIAN_POINT('Ctrl Pts',(0.0649476351123397,1.30629366210296,1.64900971937348));
#7315=CARTESIAN_POINT('Ctrl Pts',(0.0314423454288488,1.3,1.65));
#7316=CARTESIAN_POINT('Ctrl Pts',(-1.38777878078145E-17,1.3,1.65));
#7317=CARTESIAN_POINT('',(-0.25,1.55,1.63095064303001));
#7318=CARTESIAN_POINT('Ctrl Pts',(-5.55111512312578E-17,1.3,1.65));
#7319=CARTESIAN_POINT('Ctrl Pts',(-0.031442345428849,1.3,1.65));
#7320=CARTESIAN_POINT('Ctrl Pts',(-0.0649476351123398,1.30629366210296,
1.64900971937348));
#7321=CARTESIAN_POINT('Ctrl Pts',(-0.126528390765307,1.33182222741682,1.64543058688707));
#7322=CARTESIAN_POINT('Ctrl Pts',(-0.154607860978349,1.35105447038507,1.64289183246942));
#7323=CARTESIAN_POINT('Ctrl Pts',(-0.198945932189457,1.39539254159618,1.63811406745469));
#7324=CARTESIAN_POINT('Ctrl Pts',(-0.218177859368546,1.42347183818157,1.63556247215209));
#7325=CARTESIAN_POINT('Ctrl Pts',(-0.243706194926033,1.48505200040818,1.63195388134767));
#7326=CARTESIAN_POINT('Ctrl Pts',(-0.25,1.51855708359447,1.63095064303001));
#7327=CARTESIAN_POINT('Ctrl Pts',(-0.25,1.55,1.63095064303001));
#7328=CARTESIAN_POINT('Ctrl Pts',(-0.25,1.55,1.63095064303001));
#7329=CARTESIAN_POINT('Ctrl Pts',(-0.25,1.58144291640553,1.63095064303001));
#7330=CARTESIAN_POINT('Ctrl Pts',(-0.243706194926033,1.61494799959182,1.63195388134767));
#7331=CARTESIAN_POINT('Ctrl Pts',(-0.218177859368546,1.67652816181843,1.63556247215209));
#7332=CARTESIAN_POINT('Ctrl Pts',(-0.198945932189456,1.70460745840382,1.63811406745469));
#7333=CARTESIAN_POINT('Ctrl Pts',(-0.154607860978348,1.74894552961493,1.64289183246942));
#7334=CARTESIAN_POINT('Ctrl Pts',(-0.126528390765307,1.76817777258318,1.64543058688707));
#7335=CARTESIAN_POINT('Ctrl Pts',(-0.0649476351123396,1.79370633789704,
1.64900971937348));
#7336=CARTESIAN_POINT('Ctrl Pts',(-0.0314423454288488,1.8,1.65));
#7337=CARTESIAN_POINT('Ctrl Pts',(7.63278329429795E-17,1.8,1.65));
#7338=CARTESIAN_POINT('Origin',(0.,1.55,0.));
#7339=CARTESIAN_POINT('',(-0.713525491562421,1.55,0.700629269222037));
#7340=CARTESIAN_POINT('',(0.125,1.55,0.21650635094611));
#7341=CARTESIAN_POINT('Ctrl Pts',(-0.713525491562421,1.55,0.700629269222037));
#7342=CARTESIAN_POINT('Ctrl Pts',(-0.713525491562421,1.5815373526696,0.700629269222037));
#7343=CARTESIAN_POINT('Ctrl Pts',(-0.718163997970498,1.61508042700263,0.695997784676727));
#7344=CARTESIAN_POINT('Ctrl Pts',(-0.73619249062986,1.67663267125761,0.676899590973058));
#7345=CARTESIAN_POINT('Ctrl Pts',(-0.749495710301795,1.70465411363682,0.662390652284073));
#7346=CARTESIAN_POINT('Ctrl Pts',(-0.778498278845144,1.74889618382539,0.628048950774009));
#7347=CARTESIAN_POINT('Ctrl Pts',(-0.796153444118959,1.76811531482682,0.605884303066698));
#7348=CARTESIAN_POINT('Ctrl Pts',(-0.832065554235658,1.79367084275751,0.555538485325663));
#7349=CARTESIAN_POINT('Ctrl Pts',(-0.850258932191534,1.8,0.527308329855002));
#7350=CARTESIAN_POINT('Ctrl Pts',(-0.881791875377343,1.8,0.472691670144998));
#7351=CARTESIAN_POINT('Ctrl Pts',(-0.897143218189782,1.79367084275751,0.442820664919227));
#7352=CARTESIAN_POINT('Ctrl Pts',(-0.92278792026947,1.76811531482682,0.386546956384144));
#7353=CARTESIAN_POINT('Ctrl Pts',(-0.933155485613026,1.74889618382539,0.360174810895352));
#7354=CARTESIAN_POINT('Ctrl Pts',(-0.948394987258249,1.70465411363682,0.31788699900678));
#7355=CARTESIAN_POINT('Ctrl Pts',(-0.954308486908894,1.67663267125761,0.299111603474267));
#7356=CARTESIAN_POINT('Ctrl Pts',(-0.961833761492987,1.61508042700263,0.273949373987484));
#7357=CARTESIAN_POINT('Ctrl Pts',(-0.963525491562421,1.5815373526696,0.267616567329817));
#7358=CARTESIAN_POINT('Ctrl Pts',(-0.963525491562421,1.5184626473304,0.267616567329817));
#7359=CARTESIAN_POINT('Ctrl Pts',(-0.961833761492987,1.48491957299737,0.273949373987484));
#7360=CARTESIAN_POINT('Ctrl Pts',(-0.954308486908894,1.42336732874239,0.299111603474267));
#7361=CARTESIAN_POINT('Ctrl Pts',(-0.948394987258249,1.39534588636318,0.31788699900678));
#7362=CARTESIAN_POINT('Ctrl Pts',(-0.933155485613026,1.35110381617461,0.360174810895352));
#7363=CARTESIAN_POINT('Ctrl Pts',(-0.92278792026947,1.33188468517318,0.386546956384144));
#7364=CARTESIAN_POINT('Ctrl Pts',(-0.897143218189782,1.30632915724249,0.442820664919227));
#7365=CARTESIAN_POINT('Ctrl Pts',(-0.881791875377343,1.3,0.472691670144998));
#7366=CARTESIAN_POINT('Ctrl Pts',(-0.850258932191534,1.3,0.527308329855002));
#7367=CARTESIAN_POINT('Ctrl Pts',(-0.832065554235658,1.30632915724249,0.555538485325663));
#7368=CARTESIAN_POINT('Ctrl Pts',(-0.796153444118959,1.33188468517318,0.605884303066698));
#7369=CARTESIAN_POINT('Ctrl Pts',(-0.778498278845144,1.35110381617461,0.628048950774009));
#7370=CARTESIAN_POINT('Ctrl Pts',(-0.749495710301795,1.39534588636318,0.662390652284073));
#7371=CARTESIAN_POINT('Ctrl Pts',(-0.73619249062986,1.42336732874239,0.676899590973058));
#7372=CARTESIAN_POINT('Ctrl Pts',(-0.718163997970498,1.48491957299737,0.695997784676727));
#7373=CARTESIAN_POINT('Ctrl Pts',(-0.713525491562421,1.5184626473304,0.700629269222037));
#7374=CARTESIAN_POINT('Ctrl Pts',(-0.713525491562421,1.55,0.700629269222037));
#7375=CARTESIAN_POINT('Origin',(0.,1.55,0.));
#7376=CARTESIAN_POINT('',(0.963525491562421,1.55,-0.267616567329817));
#7377=CARTESIAN_POINT('Ctrl Pts',(0.963525491562421,1.55,-0.267616567329817));
#7378=CARTESIAN_POINT('Ctrl Pts',(0.963525491562421,1.5184626473304,-0.267616567329817));
#7379=CARTESIAN_POINT('Ctrl Pts',(0.961833761492987,1.48491957299737,-0.273949373987484));
#7380=CARTESIAN_POINT('Ctrl Pts',(0.954308486908894,1.42336732874239,-0.299111603474267));
#7381=CARTESIAN_POINT('Ctrl Pts',(0.948394987258249,1.39534588636318,-0.31788699900678));
#7382=CARTESIAN_POINT('Ctrl Pts',(0.933155485613026,1.35110381617461,-0.360174810895352));
#7383=CARTESIAN_POINT('Ctrl Pts',(0.92278792026947,1.33188468517318,-0.386546956384144));
#7384=CARTESIAN_POINT('Ctrl Pts',(0.897143218189782,1.30632915724249,-0.442820664919227));
#7385=CARTESIAN_POINT('Ctrl Pts',(0.881791875377343,1.3,-0.472691670144998));
#7386=CARTESIAN_POINT('Ctrl Pts',(0.850258932191534,1.3,-0.527308329855002));
#7387=CARTESIAN_POINT('Ctrl Pts',(0.832065554235658,1.30632915724249,-0.555538485325663));
#7388=CARTESIAN_POINT('Ctrl Pts',(0.796153444118959,1.33188468517318,-0.605884303066698));
#7389=CARTESIAN_POINT('Ctrl Pts',(0.778498278845144,1.35110381617461,-0.628048950774009));
#7390=CARTESIAN_POINT('Ctrl Pts',(0.749495710301795,1.39534588636318,-0.662390652284073));
#7391=CARTESIAN_POINT('Ctrl Pts',(0.73619249062986,1.42336732874239,-0.676899590973058));
#7392=CARTESIAN_POINT('Ctrl Pts',(0.718163997970498,1.48491957299737,-0.695997784676727));
#7393=CARTESIAN_POINT('Ctrl Pts',(0.713525491562421,1.5184626473304,-0.700629269222037));
#7394=CARTESIAN_POINT('Ctrl Pts',(0.713525491562421,1.5815373526696,-0.700629269222037));
#7395=CARTESIAN_POINT('Ctrl Pts',(0.718163997970498,1.61508042700263,-0.695997784676727));
#7396=CARTESIAN_POINT('Ctrl Pts',(0.73619249062986,1.67663267125761,-0.676899590973058));
#7397=CARTESIAN_POINT('Ctrl Pts',(0.749495710301795,1.70465411363682,-0.662390652284073));
#7398=CARTESIAN_POINT('Ctrl Pts',(0.778498278845144,1.74889618382539,-0.628048950774009));
#7399=CARTESIAN_POINT('Ctrl Pts',(0.796153444118959,1.76811531482682,-0.605884303066698));
#7400=CARTESIAN_POINT('Ctrl Pts',(0.832065554235658,1.79367084275751,-0.555538485325663));
#7401=CARTESIAN_POINT('Ctrl Pts',(0.850258932191534,1.8,-0.527308329855002));
#7402=CARTESIAN_POINT('Ctrl Pts',(0.881791875377343,1.8,-0.472691670144998));
#7403=CARTESIAN_POINT('Ctrl Pts',(0.897143218189782,1.79367084275751,-0.442820664919227));
#7404=CARTESIAN_POINT('Ctrl Pts',(0.92278792026947,1.76811531482682,-0.386546956384144));
#7405=CARTESIAN_POINT('Ctrl Pts',(0.933155485613026,1.74889618382539,-0.360174810895352));
#7406=CARTESIAN_POINT('Ctrl Pts',(0.948394987258249,1.70465411363682,-0.31788699900678));
#7407=CARTESIAN_POINT('Ctrl Pts',(0.954308486908894,1.67663267125761,-0.299111603474267));
#7408=CARTESIAN_POINT('Ctrl Pts',(0.961833761492987,1.61508042700263,-0.273949373987484));
#7409=CARTESIAN_POINT('Ctrl Pts',(0.963525491562421,1.5815373526696,-0.267616567329817));
#7410=CARTESIAN_POINT('Ctrl Pts',(0.963525491562421,1.55,-0.267616567329817));
#7411=CARTESIAN_POINT('',(0.125,1.55,0.21650635094611));
#7412=CARTESIAN_POINT('Origin',(0.,1.55,0.));
#7413=CARTESIAN_POINT('',(-0.25,1.55,-0.968245836551854));
#7414=CARTESIAN_POINT('',(-0.25,1.55,0.));
#7415=CARTESIAN_POINT('Ctrl Pts',(-0.25,1.55,-0.968245836551854));
#7416=CARTESIAN_POINT('Ctrl Pts',(-0.25,1.5815373526696,-0.968245836551854));
#7417=CARTESIAN_POINT('Ctrl Pts',(-0.243669763522489,1.61508042700263,-0.969947158664211));
#7418=CARTESIAN_POINT('Ctrl Pts',(-0.218115996279034,1.67663267125761,-0.976011194447325));
#7419=CARTESIAN_POINT('Ctrl Pts',(-0.198899276956455,1.70465411363682,-0.980277651290853));
#7420=CARTESIAN_POINT('Ctrl Pts',(-0.154657206767882,1.74889618382539,-0.988223761669361));
#7421=CARTESIAN_POINT('Ctrl Pts',(-0.126634476150511,1.76811531482682,-0.992431259450842));
#7422=CARTESIAN_POINT('Ctrl Pts',(-0.0650776639541238,1.79367084275751,
-0.99835915024489));
#7423=CARTESIAN_POINT('Ctrl Pts',(-0.0315329431858092,1.8,-1.));
#7424=CARTESIAN_POINT('Ctrl Pts',(0.0315329431858092,1.8,-1.));
#7425=CARTESIAN_POINT('Ctrl Pts',(0.0650776639541238,1.79367084275751,-0.99835915024489));
#7426=CARTESIAN_POINT('Ctrl Pts',(0.126634476150511,1.76811531482682,-0.992431259450842));
#7427=CARTESIAN_POINT('Ctrl Pts',(0.154657206767882,1.74889618382539,-0.988223761669361));
#7428=CARTESIAN_POINT('Ctrl Pts',(0.198899276956455,1.70465411363682,-0.980277651290853));
#7429=CARTESIAN_POINT('Ctrl Pts',(0.218115996279034,1.67663267125761,-0.976011194447325));
#7430=CARTESIAN_POINT('Ctrl Pts',(0.243669763522488,1.61508042700263,-0.969947158664211));
#7431=CARTESIAN_POINT('Ctrl Pts',(0.25,1.5815373526696,-0.968245836551854));
#7432=CARTESIAN_POINT('Ctrl Pts',(0.25,1.5184626473304,-0.968245836551854));
#7433=CARTESIAN_POINT('Ctrl Pts',(0.243669763522488,1.48491957299737,-0.969947158664211));
#7434=CARTESIAN_POINT('Ctrl Pts',(0.218115996279034,1.42336732874239,-0.976011194447325));
#7435=CARTESIAN_POINT('Ctrl Pts',(0.198899276956455,1.39534588636318,-0.980277651290853));
#7436=CARTESIAN_POINT('Ctrl Pts',(0.154657206767882,1.35110381617461,-0.988223761669361));
#7437=CARTESIAN_POINT('Ctrl Pts',(0.126634476150511,1.33188468517318,-0.992431259450842));
#7438=CARTESIAN_POINT('Ctrl Pts',(0.0650776639541239,1.30632915724249,-0.99835915024489));
#7439=CARTESIAN_POINT('Ctrl Pts',(0.0315329431858092,1.3,-1.));
#7440=CARTESIAN_POINT('Ctrl Pts',(-0.0315329431858092,1.3,-1.));
#7441=CARTESIAN_POINT('Ctrl Pts',(-0.0650776639541239,1.30632915724249,
-0.99835915024489));
#7442=CARTESIAN_POINT('Ctrl Pts',(-0.126634476150511,1.33188468517318,-0.992431259450842));
#7443=CARTESIAN_POINT('Ctrl Pts',(-0.154657206767882,1.35110381617461,-0.988223761669361));
#7444=CARTESIAN_POINT('Ctrl Pts',(-0.198899276956455,1.39534588636318,-0.980277651290853));
#7445=CARTESIAN_POINT('Ctrl Pts',(-0.218115996279034,1.42336732874239,-0.976011194447325));
#7446=CARTESIAN_POINT('Ctrl Pts',(-0.243669763522489,1.48491957299737,-0.969947158664211));
#7447=CARTESIAN_POINT('Ctrl Pts',(-0.25,1.5184626473304,-0.968245836551854));
#7448=CARTESIAN_POINT('Ctrl Pts',(-0.25,1.55,-0.968245836551854));
#7449=CARTESIAN_POINT('Origin',(0.,1.55,0.));
#7450=CARTESIAN_POINT('',(-0.25,1.55,0.968245836551854));
#7451=CARTESIAN_POINT('Ctrl Pts',(-0.25,1.55,0.968245836551854));
#7452=CARTESIAN_POINT('Ctrl Pts',(-0.25,1.5184626473304,0.968245836551854));
#7453=CARTESIAN_POINT('Ctrl Pts',(-0.243669763522489,1.48491957299737,0.969947158664211));
#7454=CARTESIAN_POINT('Ctrl Pts',(-0.218115996279034,1.42336732874239,0.976011194447325));
#7455=CARTESIAN_POINT('Ctrl Pts',(-0.198899276956455,1.39534588636318,0.980277651290853));
#7456=CARTESIAN_POINT('Ctrl Pts',(-0.154657206767882,1.35110381617461,0.988223761669361));
#7457=CARTESIAN_POINT('Ctrl Pts',(-0.126634476150511,1.33188468517318,0.992431259450842));
#7458=CARTESIAN_POINT('Ctrl Pts',(-0.065077663954124,1.30632915724249,0.99835915024489));
#7459=CARTESIAN_POINT('Ctrl Pts',(-0.0315329431858092,1.3,1.));
#7460=CARTESIAN_POINT('Ctrl Pts',(0.0315329431858092,1.3,1.));
#7461=CARTESIAN_POINT('Ctrl Pts',(0.065077663954124,1.30632915724249,0.99835915024489));
#7462=CARTESIAN_POINT('Ctrl Pts',(0.126634476150511,1.33188468517318,0.992431259450842));
#7463=CARTESIAN_POINT('Ctrl Pts',(0.154657206767882,1.35110381617461,0.988223761669361));
#7464=CARTESIAN_POINT('Ctrl Pts',(0.198899276956455,1.39534588636318,0.980277651290853));
#7465=CARTESIAN_POINT('Ctrl Pts',(0.218115996279034,1.42336732874239,0.976011194447325));
#7466=CARTESIAN_POINT('Ctrl Pts',(0.243669763522488,1.48491957299737,0.969947158664211));
#7467=CARTESIAN_POINT('Ctrl Pts',(0.25,1.5184626473304,0.968245836551854));
#7468=CARTESIAN_POINT('Ctrl Pts',(0.25,1.5815373526696,0.968245836551854));
#7469=CARTESIAN_POINT('Ctrl Pts',(0.243669763522488,1.61508042700263,0.969947158664211));
#7470=CARTESIAN_POINT('Ctrl Pts',(0.218115996279034,1.67663267125761,0.976011194447325));
#7471=CARTESIAN_POINT('Ctrl Pts',(0.198899276956455,1.70465411363682,0.980277651290853));
#7472=CARTESIAN_POINT('Ctrl Pts',(0.154657206767882,1.74889618382539,0.988223761669361));
#7473=CARTESIAN_POINT('Ctrl Pts',(0.126634476150511,1.76811531482682,0.992431259450842));
#7474=CARTESIAN_POINT('Ctrl Pts',(0.0650776639541239,1.79367084275751,0.99835915024489));
#7475=CARTESIAN_POINT('Ctrl Pts',(0.0315329431858092,1.8,1.));
#7476=CARTESIAN_POINT('Ctrl Pts',(-0.0315329431858092,1.8,1.));
#7477=CARTESIAN_POINT('Ctrl Pts',(-0.0650776639541239,1.79367084275751,
0.99835915024489));
#7478=CARTESIAN_POINT('Ctrl Pts',(-0.126634476150511,1.76811531482682,0.992431259450842));
#7479=CARTESIAN_POINT('Ctrl Pts',(-0.154657206767882,1.74889618382539,0.988223761669361));
#7480=CARTESIAN_POINT('Ctrl Pts',(-0.198899276956455,1.70465411363682,0.980277651290853));
#7481=CARTESIAN_POINT('Ctrl Pts',(-0.218115996279034,1.67663267125761,0.976011194447325));
#7482=CARTESIAN_POINT('Ctrl Pts',(-0.243669763522489,1.61508042700263,0.969947158664211));
#7483=CARTESIAN_POINT('Ctrl Pts',(-0.25,1.5815373526696,0.968245836551854));
#7484=CARTESIAN_POINT('Ctrl Pts',(-0.25,1.55,0.968245836551854));
#7485=CARTESIAN_POINT('',(-0.25,1.55,0.));
#7486=CARTESIAN_POINT('Origin',(1.65,2.25,0.));
#7487=CARTESIAN_POINT('',(-1.,2.25,-1.22464679914735E-16));
#7488=CARTESIAN_POINT('Origin',(0.,2.25,0.));
#7489=CARTESIAN_POINT('Origin',(1.75,0.85,0.));
#7490=CARTESIAN_POINT('',(-1.75,0.85,-2.14313189850787E-16));
#7491=CARTESIAN_POINT('Origin',(0.,0.85,0.));
#7492=CARTESIAN_POINT('Origin',(0.,0.,0.));
#7493=CARTESIAN_POINT('',(-1.75,-0.85,-2.14313189850787E-16));
#7494=CARTESIAN_POINT('Origin',(0.,-0.85,0.));
#7495=CARTESIAN_POINT('',(-1.75,0.,-2.14313189850787E-16));
#7496=CARTESIAN_POINT('Origin',(1.,-0.85,0.));
#7497=CARTESIAN_POINT('',(-1.,-0.85,-1.22464679914735E-16));
#7498=CARTESIAN_POINT('Origin',(0.,-0.85,0.));
#7499=CARTESIAN_POINT('Origin',(0.,0.7,0.));
#7500=CARTESIAN_POINT('',(-1.,0.7,-1.22464679914735E-16));
#7501=CARTESIAN_POINT('',(0.,0.,0.));
#7502=CARTESIAN_POINT('',(0.,0.,0.));
#7503=CARTESIAN_POINT('',(0.,0.,0.));
#7504=CARTESIAN_POINT('Origin',(0.,0.,0.));
#7505=CARTESIAN_POINT('',(-0.42,0.16,5.14351655641888E-17));
#7506=CARTESIAN_POINT('Origin',(0.,0.16,0.));
#7507=CARTESIAN_POINT('',(-0.42,0.,5.14351655641888E-17));
#7508=CARTESIAN_POINT('',(-0.42,0.,5.14351655641888E-17));
#7509=CARTESIAN_POINT('Origin',(0.,0.,0.));
#7510=CARTESIAN_POINT('Origin',(0.,0.,0.));
#7511=CARTESIAN_POINT('',(-0.8,0.16,9.79717439317883E-17));
#7512=CARTESIAN_POINT('Origin',(0.,0.16,0.));
#7513=CARTESIAN_POINT('',(-0.8,0.,9.79717439317883E-17));
#7514=CARTESIAN_POINT('',(-0.8,0.,9.79717439317883E-17));
#7515=CARTESIAN_POINT('Origin',(0.,0.,0.));
#7516=CARTESIAN_POINT('Origin',(0.,0.16,0.));
#7517=CARTESIAN_POINT('Origin',(0.,0.,0.));
#7518=CARTESIAN_POINT('',(0.,0.,0.));
#7519=CARTESIAN_POINT('Origin',(0.173205080756888,-0.8,-0.3));
#7520=CARTESIAN_POINT('',(0.346410161513775,-0.8,0.));
#7521=CARTESIAN_POINT('',(0.173205080756888,-0.8,-0.3));
#7522=CARTESIAN_POINT('',(0.346410161513775,-0.8,0.));
#7523=CARTESIAN_POINT('',(0.173205080756888,-1.28,-0.3));
#7524=CARTESIAN_POINT('',(0.173205080756888,-0.8,-0.3));
#7525=CARTESIAN_POINT('',(0.346410161513775,-1.28,0.));
#7526=CARTESIAN_POINT('',(0.346410161513775,-1.28,0.));
#7527=CARTESIAN_POINT('',(0.346410161513775,-0.8,0.));
#7528=CARTESIAN_POINT('Origin',(-0.173205080756888,-0.8,-0.3));
#7529=CARTESIAN_POINT('',(-0.173205080756888,-0.8,-0.3));
#7530=CARTESIAN_POINT('',(0.173205080756888,-0.8,-0.3));
#7531=CARTESIAN_POINT('',(-0.173205080756888,-1.28,-0.3));
#7532=CARTESIAN_POINT('',(-0.173205080756888,-0.8,-0.3));
#7533=CARTESIAN_POINT('',(0.173205080756888,-1.28,-0.3));
#7534=CARTESIAN_POINT('Origin',(-0.346410161513775,-0.8,-5.55111512312578E-17));
#7535=CARTESIAN_POINT('',(-0.346410161513775,-0.8,-4.24230095489963E-17));
#7536=CARTESIAN_POINT('',(-0.173205080756888,-0.8,-0.3));
#7537=CARTESIAN_POINT('',(-0.346410161513775,-1.28,-5.55111512312578E-17));
#7538=CARTESIAN_POINT('',(-0.346410161513775,-0.8,-4.24230095489963E-17));
#7539=CARTESIAN_POINT('',(-0.173205080756888,-1.28,-0.3));
#7540=CARTESIAN_POINT('Origin',(-0.173205080756888,-0.8,0.3));
#7541=CARTESIAN_POINT('',(-0.173205080756888,-0.8,0.3));
#7542=CARTESIAN_POINT('',(-0.346410161513775,-0.8,-4.24230095489963E-17));
#7543=CARTESIAN_POINT('',(-0.173205080756888,-1.28,0.3));
#7544=CARTESIAN_POINT('',(-0.173205080756888,-0.8,0.3));
#7545=CARTESIAN_POINT('',(-0.346410161513775,-1.28,-4.24230095489963E-17));
#7546=CARTESIAN_POINT('Origin',(0.173205080756888,-0.8,0.3));
#7547=CARTESIAN_POINT('',(0.173205080756888,-0.8,0.3));
#7548=CARTESIAN_POINT('',(-0.173205080756888,-0.8,0.3));
#7549=CARTESIAN_POINT('',(0.173205080756888,-1.28,0.3));
#7550=CARTESIAN_POINT('',(0.173205080756888,-0.8,0.3));
#7551=CARTESIAN_POINT('',(-0.173205080756888,-1.28,0.3));
#7552=CARTESIAN_POINT('Origin',(0.346410161513775,-0.8,0.));
#7553=CARTESIAN_POINT('',(0.173205080756888,-0.8,0.3));
#7554=CARTESIAN_POINT('',(0.173205080756888,-1.28,0.3));
#7555=CARTESIAN_POINT('Origin',(0.,-0.8,-5.55111512312578E-17));
#7556=CARTESIAN_POINT('Origin',(0.,-1.28,-5.55111512312578E-17));
#7557=CARTESIAN_POINT('Origin',(0.,-2.5,0.));
#7558=CARTESIAN_POINT('',(-0.3933,-2.5,4.81653586104654E-17));
#7559=CARTESIAN_POINT('Origin',(0.,-2.5,0.));
#7560=CARTESIAN_POINT('Origin',(0.6,0.8,0.));
#7561=CARTESIAN_POINT('',(-0.6,0.8,-7.34788079488412E-17));
#7562=CARTESIAN_POINT('Origin',(0.,0.8,0.));
#7563=CARTESIAN_POINT('Origin',(0.,0.775,0.));
#7564=CARTESIAN_POINT('',(-0.65,0.75,-7.9602041944578E-17));
#7565=CARTESIAN_POINT('Origin',(0.,0.75,0.));
#7566=CARTESIAN_POINT('',(-0.625,0.775,-7.65404249467096E-17));
#7567=CARTESIAN_POINT('Origin',(0.,0.39,0.));
#7568=CARTESIAN_POINT('',(-0.65,0.0299999999999998,-7.9602041944578E-17));
#7569=CARTESIAN_POINT('Origin',(0.,0.0299999999999998,0.));
#7570=CARTESIAN_POINT('',(-0.65,0.39,-7.9602041944578E-17));
#7571=CARTESIAN_POINT('Origin',(0.,0.0150000000000001,0.));
#7572=CARTESIAN_POINT('',(-0.62,5.89805981832114E-17,-7.59281015471359E-17));
#7573=CARTESIAN_POINT('Origin',(0.,0.,0.));
#7574=CARTESIAN_POINT('',(-0.635,0.0150000000000001,-7.77650717458569E-17));
#7575=CARTESIAN_POINT('Origin',(0.42,0.,0.));
#7576=CARTESIAN_POINT('',(-0.42,-3.46944695195361E-18,-5.14351655641888E-17));
#7577=CARTESIAN_POINT('Origin',(0.,0.,0.));
#7578=CARTESIAN_POINT('Origin',(0.,-0.02,0.));
#7579=CARTESIAN_POINT('',(-0.3933,-0.0534000000000001,4.81653586104654E-17));
#7580=CARTESIAN_POINT('Origin',(0.,-0.0534000000000001,0.));
#7581=CARTESIAN_POINT('',(-0.41,-0.02,-5.02105187650415E-17));
#7582=CARTESIAN_POINT('Origin',(0.,-1.48,0.));
#7583=CARTESIAN_POINT('',(-0.3933,-1.48,-4.81653586104654E-17));
#7584=CARTESIAN_POINT('',(0.,0.,0.));
#7585=CARTESIAN_POINT('',(0.,0.,0.));
#7586=CARTESIAN_POINT('',(0.,0.,0.));
#7587=CARTESIAN_POINT('',(0.,0.,0.));
#7588=CARTESIAN_POINT('',(0.,0.,0.));
#7589=CARTESIAN_POINT('',(0.,0.,0.));
#7590=CARTESIAN_POINT('',(0.,0.,0.));
#7591=CARTESIAN_POINT('',(0.,0.,0.));
#7592=CARTESIAN_POINT('',(0.,0.,0.));
#7593=CARTESIAN_POINT('',(0.,0.,0.));
#7594=CARTESIAN_POINT('',(0.,0.,0.));
#7595=CARTESIAN_POINT('',(-6.,-3.,1.2));
#7596=CARTESIAN_POINT('',(-6.,-3.,1.36));
#7597=CARTESIAN_POINT('',(6.,-3.,1.2));
#7598=CARTESIAN_POINT('',(6.,-3.,1.36));
#7599=CARTESIAN_POINT('',(-6.,33.,1.2));
#7600=CARTESIAN_POINT('',(-6.,33.,1.36));
#7601=CARTESIAN_POINT('',(6.,33.,1.2));
#7602=CARTESIAN_POINT('',(6.,33.,1.36));
#7603=CARTESIAN_POINT('',(0.,0.,4.53));
#7604=CARTESIAN_POINT('',(-4.75,0.,2.4));
#7605=CARTESIAN_POINT('',(-4.75,0.,2.56));
#7606=CARTESIAN_POINT('',(4.75,0.,2.4));
#7607=CARTESIAN_POINT('',(4.75,0.,2.56));
#7608=CARTESIAN_POINT('',(0.,15.,4.53));
#7609=CARTESIAN_POINT('',(-4.75,15.,2.4));
#7610=CARTESIAN_POINT('',(-4.75,15.,2.56));
#7611=CARTESIAN_POINT('',(4.75,15.,2.4));
#7612=CARTESIAN_POINT('',(4.75,15.,2.56));
#7613=CARTESIAN_POINT('',(0.,30.,4.53));
#7614=CARTESIAN_POINT('',(-4.75,30.,2.4));
#7615=CARTESIAN_POINT('',(-4.75,30.,2.56));
#7616=CARTESIAN_POINT('',(4.75,30.,2.4));
#7617=CARTESIAN_POINT('',(4.75,30.,2.56));
#7618=CARTESIAN_POINT('',(0.,0.,0.));
#7619=CARTESIAN_POINT('',(0.,0.,0.));
#7620=CARTESIAN_POINT('Origin',(0.,32.5,4.53));
#7621=CARTESIAN_POINT('',(-0.21,32.5,4.53));
#7622=CARTESIAN_POINT('Origin',(0.,32.5,4.53));
#7623=CARTESIAN_POINT('',(-0.21,34.5,4.53));
#7624=CARTESIAN_POINT('',(-0.21,32.5,4.53));
#7625=CARTESIAN_POINT('Origin',(0.,34.5,4.53));
#7626=CARTESIAN_POINT('Origin',(0.,32.5,4.53));
#7627=CARTESIAN_POINT('Origin',(0.,-4.6,4.53));
#7628=CARTESIAN_POINT('',(-0.21,-4.5,4.53));
#7629=CARTESIAN_POINT('Origin',(0.,-4.5,4.53));
#7630=CARTESIAN_POINT('',(-0.21,-2.5,4.53));
#7631=CARTESIAN_POINT('',(-0.21,-4.6,4.53));
#7632=CARTESIAN_POINT('Origin',(0.,-2.5,4.53));
#7633=CARTESIAN_POINT('Origin',(0.,-2.5,4.53));
#7634=CARTESIAN_POINT('Origin',(-0.3,21.,3.4));
#7635=CARTESIAN_POINT('',(-0.3,23.5,3.57606079858305));
#7636=CARTESIAN_POINT('',(-0.3,21.,3.57606079858305));
#7637=CARTESIAN_POINT('',(-0.3,-4.5,3.57606079858305));
#7638=CARTESIAN_POINT('',(-0.3,23.5,3.88));
#7639=CARTESIAN_POINT('',(-0.3,23.5,3.88));
#7640=CARTESIAN_POINT('',(-0.3,21.,3.88));
#7641=CARTESIAN_POINT('',(-0.3,21.,3.88));
#7642=CARTESIAN_POINT('',(-0.3,21.,3.88));
#7643=CARTESIAN_POINT('Origin',(0.,21.,3.64));
#7644=CARTESIAN_POINT('',(0.3,21.,3.57606079858305));
#7645=CARTESIAN_POINT('Origin',(0.,21.,4.53));
#7646=CARTESIAN_POINT('',(0.3,21.,3.88));
#7647=CARTESIAN_POINT('',(0.3,21.,3.88));
#7648=CARTESIAN_POINT('',(0.3,21.,3.4));
#7649=CARTESIAN_POINT('Origin',(0.3,21.,3.88));
#7650=CARTESIAN_POINT('',(0.3,23.5,3.57606079858305));
#7651=CARTESIAN_POINT('',(0.3,-4.5,3.57606079858305));
#7652=CARTESIAN_POINT('',(0.3,23.5,3.88));
#7653=CARTESIAN_POINT('',(0.3,21.,3.88));
#7654=CARTESIAN_POINT('',(0.3,23.5,3.4));
#7655=CARTESIAN_POINT('Origin',(-0.3,21.,3.88));
#7656=CARTESIAN_POINT('',(0.3,23.5,3.88));
#7657=CARTESIAN_POINT('Origin',(0.,23.5,3.64));
#7658=CARTESIAN_POINT('Origin',(0.,23.5,4.53));
#7659=CARTESIAN_POINT('Origin',(-0.3,6.,3.4));
#7660=CARTESIAN_POINT('',(-0.3,8.5,3.57606079858305));
#7661=CARTESIAN_POINT('',(-0.3,6.,3.57606079858305));
#7662=CARTESIAN_POINT('',(-0.3,-4.5,3.57606079858305));
#7663=CARTESIAN_POINT('',(-0.3,8.5,3.88));
#7664=CARTESIAN_POINT('',(-0.3,8.5,3.88));
#7665=CARTESIAN_POINT('',(-0.3,6.,3.88));
#7666=CARTESIAN_POINT('',(-0.3,6.,3.88));
#7667=CARTESIAN_POINT('',(-0.3,6.,3.88));
#7668=CARTESIAN_POINT('Origin',(0.,6.,3.64));
#7669=CARTESIAN_POINT('',(0.3,6.,3.57606079858305));
#7670=CARTESIAN_POINT('Origin',(0.,6.,4.53));
#7671=CARTESIAN_POINT('',(0.3,6.,3.88));
#7672=CARTESIAN_POINT('',(0.3,6.,3.88));
#7673=CARTESIAN_POINT('',(0.3,6.,3.4));
#7674=CARTESIAN_POINT('Origin',(0.3,6.,3.88));
#7675=CARTESIAN_POINT('',(0.3,8.5,3.57606079858305));
#7676=CARTESIAN_POINT('',(0.3,-4.5,3.57606079858305));
#7677=CARTESIAN_POINT('',(0.3,8.5,3.88));
#7678=CARTESIAN_POINT('',(0.3,6.,3.88));
#7679=CARTESIAN_POINT('',(0.3,8.5,3.4));
#7680=CARTESIAN_POINT('Origin',(-0.3,6.,3.88));
#7681=CARTESIAN_POINT('',(0.3,8.5,3.88));
#7682=CARTESIAN_POINT('Origin',(0.,8.5,3.64));
#7683=CARTESIAN_POINT('Origin',(0.,8.5,4.53));
#7684=CARTESIAN_POINT('Origin',(0.,-4.5,4.53));
#7685=CARTESIAN_POINT('',(-1.,34.5,4.53));
#7686=CARTESIAN_POINT('Origin',(0.,34.5,4.53));
#7687=CARTESIAN_POINT('',(-1.,-4.5,4.53));
#7688=CARTESIAN_POINT('',(-1.,-4.5,4.53));
#7689=CARTESIAN_POINT('Origin',(0.,-4.5,4.53));
#7690=CARTESIAN_POINT('Origin',(0.,34.5,4.53));
#7691=CARTESIAN_POINT('Origin',(0.,-4.5,4.53));
#7692=CARTESIAN_POINT('',(0.,0.,0.));
#7693=CARTESIAN_POINT('Origin',(0.,7.25,5.52));
#7694=CARTESIAN_POINT('',(0.141067359796651,7.09443650813895,5.52));
#7695=CARTESIAN_POINT('',(0.141067359796651,7.40556349186105,5.52));
#7696=CARTESIAN_POINT('',(0.141067359796651,6.,5.52));
#7697=CARTESIAN_POINT('Origin',(0.,7.25,5.52));
#7698=CARTESIAN_POINT('Origin',(0.,7.25,5.52));
#7699=CARTESIAN_POINT('',(-0.141067359796651,7.09443650813895,5.52));
#7700=CARTESIAN_POINT('Ctrl Pts',(-0.141067359796651,7.09443650813895,5.52));
#7701=CARTESIAN_POINT('Ctrl Pts',(-0.12381835669822,7.0787948476368,5.52245784982447));
#7702=CARTESIAN_POINT('Ctrl Pts',(-0.102998643109696,7.06537595666898,5.52493819304946));
#7703=CARTESIAN_POINT('Ctrl Pts',(-0.0546141143983527,7.04530253627557,
5.52884449237241));
#7704=CARTESIAN_POINT('Ctrl Pts',(-0.0264520736824499,7.04,5.53));
#7705=CARTESIAN_POINT('Ctrl Pts',(0.0264520736824498,7.04,5.53));
#7706=CARTESIAN_POINT('Ctrl Pts',(0.0546141143983529,7.04530253627557,5.52884449237241));
#7707=CARTESIAN_POINT('Ctrl Pts',(0.102998643109696,7.06537595666898,5.52493819304946));
#7708=CARTESIAN_POINT('Ctrl Pts',(0.123818356698219,7.0787948476368,5.52245784982447));
#7709=CARTESIAN_POINT('Ctrl Pts',(0.141067359796651,7.09443650813895,5.52));
#7710=CARTESIAN_POINT('',(-0.21,7.25,5.52));
#7711=CARTESIAN_POINT('Origin',(0.,7.25,5.52));
#7712=CARTESIAN_POINT('',(-0.21,7.25,6.51894444366855));
#7713=CARTESIAN_POINT('',(-0.21,7.25,5.52));
#7714=CARTESIAN_POINT('',(0.21,7.25,6.51894444366855));
#7715=CARTESIAN_POINT('Ctrl Pts',(0.21,7.25,6.51894444366855));
#7716=CARTESIAN_POINT('Ctrl Pts',(0.21,7.22361099164069,6.51894444366855));
#7717=CARTESIAN_POINT('Ctrl Pts',(0.204722164681422,7.19547640622183,6.51952376620524));
#7718=CARTESIAN_POINT('Ctrl Pts',(0.183284867450471,7.14374255317885,6.52161307432363));
#7719=CARTESIAN_POINT('Ctrl Pts',(0.167126466290584,7.12014161819223,6.52309254589373));
#7720=CARTESIAN_POINT('Ctrl Pts',(0.129858458976497,7.08287361087815,6.52586721250997));
#7721=CARTESIAN_POINT('Ctrl Pts',(0.106257490219277,7.06671514943451,6.527343117591));
#7722=CARTESIAN_POINT('Ctrl Pts',(0.054523523784787,7.04527780741314,6.52942425936951));
#7723=CARTESIAN_POINT('Ctrl Pts',(0.0263888990751171,7.04,6.53));
#7724=CARTESIAN_POINT('Ctrl Pts',(-0.0263888990751171,7.04,6.53));
#7725=CARTESIAN_POINT('Ctrl Pts',(-0.0545235237847869,7.04527780741314,
6.52942425936951));
#7726=CARTESIAN_POINT('Ctrl Pts',(-0.106257490219277,7.06671514943451,6.527343117591));
#7727=CARTESIAN_POINT('Ctrl Pts',(-0.129858458976497,7.08287361087815,6.52586721250997));
#7728=CARTESIAN_POINT('Ctrl Pts',(-0.167126466290584,7.12014161819223,6.52309254589373));
#7729=CARTESIAN_POINT('Ctrl Pts',(-0.183284867450471,7.14374255317885,6.52161307432363));
#7730=CARTESIAN_POINT('Ctrl Pts',(-0.204722164681422,7.19547640622183,6.51952376620524));
#7731=CARTESIAN_POINT('Ctrl Pts',(-0.21,7.22361099164069,6.51894444366855));
#7732=CARTESIAN_POINT('Ctrl Pts',(-0.21,7.25,6.51894444366855));
#7733=CARTESIAN_POINT('Ctrl Pts',(-0.21,7.25,6.51894444366855));
#7734=CARTESIAN_POINT('Ctrl Pts',(-0.21,7.27638900835931,6.51894444366855));
#7735=CARTESIAN_POINT('Ctrl Pts',(-0.204722164681422,7.30452359377817,6.51952376620524));
#7736=CARTESIAN_POINT('Ctrl Pts',(-0.183284867450471,7.35625744682115,6.52161307432363));
#7737=CARTESIAN_POINT('Ctrl Pts',(-0.167126466290584,7.37985838180777,6.52309254589373));
#7738=CARTESIAN_POINT('Ctrl Pts',(-0.129858458976497,7.41712638912185,6.52586721250997));
#7739=CARTESIAN_POINT('Ctrl Pts',(-0.106257490219277,7.43328485056549,6.527343117591));
#7740=CARTESIAN_POINT('Ctrl Pts',(-0.054523523784787,7.45472219258686,6.52942425936951));
#7741=CARTESIAN_POINT('Ctrl Pts',(-0.0263888990751171,7.46,6.53));
#7742=CARTESIAN_POINT('Ctrl Pts',(0.026388899075117,7.46,6.53));
#7743=CARTESIAN_POINT('Ctrl Pts',(0.0545235237847869,7.45472219258686,6.52942425936951));
#7744=CARTESIAN_POINT('Ctrl Pts',(0.106257490219278,7.43328485056549,6.527343117591));
#7745=CARTESIAN_POINT('Ctrl Pts',(0.129858458976496,7.41712638912185,6.52586721250997));
#7746=CARTESIAN_POINT('Ctrl Pts',(0.167126466290584,7.37985838180777,6.52309254589373));
#7747=CARTESIAN_POINT('Ctrl Pts',(0.183284867450471,7.35625744682115,6.52161307432363));
#7748=CARTESIAN_POINT('Ctrl Pts',(0.204722164681422,7.30452359377817,6.51952376620524));
#7749=CARTESIAN_POINT('Ctrl Pts',(0.21,7.27638900835931,6.51894444366855));
#7750=CARTESIAN_POINT('Ctrl Pts',(0.21,7.25,6.51894444366855));
#7751=CARTESIAN_POINT('',(-0.141067359796651,7.40556349186105,5.52));
#7752=CARTESIAN_POINT('Origin',(0.,7.25,5.52));
#7753=CARTESIAN_POINT('Ctrl Pts',(0.141067359796651,7.40556349186105,5.52));
#7754=CARTESIAN_POINT('Ctrl Pts',(0.123818356698219,7.4212051523632,5.52245784982447));
#7755=CARTESIAN_POINT('Ctrl Pts',(0.102998643109696,7.43462404333102,5.52493819304946));
#7756=CARTESIAN_POINT('Ctrl Pts',(0.0546141143983527,7.45469746372443,5.52884449237241));
#7757=CARTESIAN_POINT('Ctrl Pts',(0.0264520736824498,7.46,5.53));
#7758=CARTESIAN_POINT('Ctrl Pts',(-0.0264520736824498,7.46,5.53));
#7759=CARTESIAN_POINT('Ctrl Pts',(-0.0546141143983527,7.45469746372443,
5.52884449237241));
#7760=CARTESIAN_POINT('Ctrl Pts',(-0.102998643109696,7.43462404333102,5.52493819304946));
#7761=CARTESIAN_POINT('Ctrl Pts',(-0.123818356698219,7.4212051523632,5.52245784982447));
#7762=CARTESIAN_POINT('Ctrl Pts',(-0.141067359796651,7.40556349186105,5.52));
#7763=CARTESIAN_POINT('Origin',(0.,7.25,5.52));
#7764=CARTESIAN_POINT('',(-0.141067359796651,6.,5.52));
#7765=CARTESIAN_POINT('Origin',(-0.3,5.9,3.25));
#7766=CARTESIAN_POINT('',(-0.3,6.,3.25));
#7767=CARTESIAN_POINT('',(-0.3,6.,3.57606079858305));
#7768=CARTESIAN_POINT('',(-0.3,6.,3.89));
#7769=CARTESIAN_POINT('',(-0.3,8.5,3.25));
#7770=CARTESIAN_POINT('',(-0.3,5.9,3.25));
#7771=CARTESIAN_POINT('',(-0.3,8.5,3.57606079858305));
#7772=CARTESIAN_POINT('',(-0.3,8.5,3.89));
#7773=CARTESIAN_POINT('',(-0.3,6.,3.57606079858305));
#7774=CARTESIAN_POINT('Origin',(0.3,5.9,3.25));
#7775=CARTESIAN_POINT('',(0.3,6.,3.25));
#7776=CARTESIAN_POINT('',(0.15,6.,3.25));
#7777=CARTESIAN_POINT('',(0.3,8.5,3.25));
#7778=CARTESIAN_POINT('',(0.3,5.9,3.25));
#7779=CARTESIAN_POINT('',(0.15,8.5,3.25));
#7780=CARTESIAN_POINT('Origin',(0.3,5.9,4.53));
#7781=CARTESIAN_POINT('',(0.3,6.,3.57606079858305));
#7782=CARTESIAN_POINT('',(0.3,6.,4.53));
#7783=CARTESIAN_POINT('',(0.3,8.5,3.57606079858305));
#7784=CARTESIAN_POINT('',(0.3,6.,3.57606079858305));
#7785=CARTESIAN_POINT('',(0.3,8.5,4.53));
#7786=CARTESIAN_POINT('Origin',(0.,8.5,4.53));
#7787=CARTESIAN_POINT('',(-2.,8.5,4.53));
#7788=CARTESIAN_POINT('Origin',(0.,8.5,4.53));
#7789=CARTESIAN_POINT('Origin',(0.,8.5,4.53));
#7790=CARTESIAN_POINT('Origin',(0.,6.,4.53));
#7791=CARTESIAN_POINT('Origin',(0.,6.,4.53));
#7792=CARTESIAN_POINT('Origin',(0.,6.,4.53));
#7793=CARTESIAN_POINT('',(-2.,6.,4.53));
#7794=CARTESIAN_POINT('',(-2.,6.,4.53));
#7795=CARTESIAN_POINT('Origin',(0.,6.,4.53));
#7796=CARTESIAN_POINT('Origin',(0.,6.,4.53));
#7797=CARTESIAN_POINT('',(0.,0.,0.));
#7798=CARTESIAN_POINT('Origin',(0.,22.25,5.52));
#7799=CARTESIAN_POINT('',(0.141067359796651,22.094436508139,5.52));
#7800=CARTESIAN_POINT('',(0.141067359796651,22.405563491861,5.52));
#7801=CARTESIAN_POINT('',(0.141067359796651,21.,5.52));
#7802=CARTESIAN_POINT('Origin',(0.,22.25,5.52));
#7803=CARTESIAN_POINT('Origin',(0.,22.25,5.52));
#7804=CARTESIAN_POINT('',(-0.141067359796651,22.094436508139,5.52));
#7805=CARTESIAN_POINT('Ctrl Pts',(-0.141067359796651,22.094436508139,5.52));
#7806=CARTESIAN_POINT('Ctrl Pts',(-0.123818356698221,22.0787948476368,5.52245784982447));
#7807=CARTESIAN_POINT('Ctrl Pts',(-0.102998643109697,22.065375956669,5.52493819304946));
#7808=CARTESIAN_POINT('Ctrl Pts',(-0.0546141143983537,22.0453025362756,
5.52884449237241));
#7809=CARTESIAN_POINT('Ctrl Pts',(-0.02645207368245,22.04,5.53));
#7810=CARTESIAN_POINT('Ctrl Pts',(0.02645207368245,22.04,5.53));
#7811=CARTESIAN_POINT('Ctrl Pts',(0.0546141143983536,22.0453025362756,5.52884449237241));
#7812=CARTESIAN_POINT('Ctrl Pts',(0.102998643109697,22.065375956669,5.52493819304946));
#7813=CARTESIAN_POINT('Ctrl Pts',(0.123818356698218,22.0787948476368,5.52245784982447));
#7814=CARTESIAN_POINT('Ctrl Pts',(0.141067359796651,22.094436508139,5.52));
#7815=CARTESIAN_POINT('',(-0.21,22.25,5.52));
#7816=CARTESIAN_POINT('Origin',(0.,22.25,5.52));
#7817=CARTESIAN_POINT('',(-0.21,22.25,6.51894444366855));
#7818=CARTESIAN_POINT('',(-0.21,22.25,5.52));
#7819=CARTESIAN_POINT('',(0.21,22.25,6.51894444366855));
#7820=CARTESIAN_POINT('Ctrl Pts',(0.21,22.25,6.51894444366855));
#7821=CARTESIAN_POINT('Ctrl Pts',(0.21,22.2236109916407,6.51894444366855));
#7822=CARTESIAN_POINT('Ctrl Pts',(0.204722164681422,22.1954764062218,6.51952376620524));
#7823=CARTESIAN_POINT('Ctrl Pts',(0.18328486745047,22.1437425531788,6.52161307432363));
#7824=CARTESIAN_POINT('Ctrl Pts',(0.167126466290583,22.1201416181922,6.52309254589373));
#7825=CARTESIAN_POINT('Ctrl Pts',(0.129858458976496,22.0828736108781,6.52586721250997));
#7826=CARTESIAN_POINT('Ctrl Pts',(0.106257490219277,22.0667151494345,6.527343117591));
#7827=CARTESIAN_POINT('Ctrl Pts',(0.0545235237847864,22.0452778074131,6.52942425936951));
#7828=CARTESIAN_POINT('Ctrl Pts',(0.0263888990751173,22.04,6.53));
#7829=CARTESIAN_POINT('Ctrl Pts',(-0.0263888990751173,22.04,6.53));
#7830=CARTESIAN_POINT('Ctrl Pts',(-0.0545235237847876,22.0452778074131,
6.52942425936951));
#7831=CARTESIAN_POINT('Ctrl Pts',(-0.106257490219279,22.0667151494345,6.527343117591));
#7832=CARTESIAN_POINT('Ctrl Pts',(-0.129858458976496,22.0828736108781,6.52586721250997));
#7833=CARTESIAN_POINT('Ctrl Pts',(-0.167126466290583,22.1201416181922,6.52309254589373));
#7834=CARTESIAN_POINT('Ctrl Pts',(-0.18328486745047,22.1437425531788,6.52161307432363));
#7835=CARTESIAN_POINT('Ctrl Pts',(-0.204722164681422,22.1954764062218,6.51952376620524));
#7836=CARTESIAN_POINT('Ctrl Pts',(-0.21,22.2236109916407,6.51894444366855));
#7837=CARTESIAN_POINT('Ctrl Pts',(-0.21,22.25,6.51894444366855));
#7838=CARTESIAN_POINT('Ctrl Pts',(-0.21,22.25,6.51894444366855));
#7839=CARTESIAN_POINT('Ctrl Pts',(-0.21,22.2763890083593,6.51894444366855));
#7840=CARTESIAN_POINT('Ctrl Pts',(-0.204722164681422,22.3045235937782,6.51952376620524));
#7841=CARTESIAN_POINT('Ctrl Pts',(-0.18328486745047,22.3562574468212,6.52161307432363));
#7842=CARTESIAN_POINT('Ctrl Pts',(-0.167126466290583,22.3798583818078,6.52309254589373));
#7843=CARTESIAN_POINT('Ctrl Pts',(-0.129858458976496,22.4171263891219,6.52586721250997));
#7844=CARTESIAN_POINT('Ctrl Pts',(-0.106257490219277,22.4332848505655,6.527343117591));
#7845=CARTESIAN_POINT('Ctrl Pts',(-0.0545235237847864,22.4547221925869,
6.52942425936951));
#7846=CARTESIAN_POINT('Ctrl Pts',(-0.0263888990751173,22.46,6.53));
#7847=CARTESIAN_POINT('Ctrl Pts',(0.0263888990751173,22.46,6.53));
#7848=CARTESIAN_POINT('Ctrl Pts',(0.054523523784789,22.4547221925869,6.52942425936951));
#7849=CARTESIAN_POINT('Ctrl Pts',(0.106257490219279,22.4332848505655,6.527343117591));
#7850=CARTESIAN_POINT('Ctrl Pts',(0.129858458976496,22.4171263891219,6.52586721250997));
#7851=CARTESIAN_POINT('Ctrl Pts',(0.167126466290583,22.3798583818078,6.52309254589373));
#7852=CARTESIAN_POINT('Ctrl Pts',(0.183284867450474,22.3562574468211,6.52161307432363));
#7853=CARTESIAN_POINT('Ctrl Pts',(0.204722164681421,22.3045235937782,6.51952376620524));
#7854=CARTESIAN_POINT('Ctrl Pts',(0.21,22.2763890083593,6.51894444366855));
#7855=CARTESIAN_POINT('Ctrl Pts',(0.21,22.25,6.51894444366855));
#7856=CARTESIAN_POINT('',(-0.141067359796651,22.405563491861,5.52));
#7857=CARTESIAN_POINT('Origin',(0.,22.25,5.52));
#7858=CARTESIAN_POINT('Ctrl Pts',(0.141067359796648,22.405563491861,5.52));
#7859=CARTESIAN_POINT('Ctrl Pts',(0.123818356698219,22.4212051523632,5.52245784982446));
#7860=CARTESIAN_POINT('Ctrl Pts',(0.102998643109699,22.434624043331,5.52493819304946));
#7861=CARTESIAN_POINT('Ctrl Pts',(0.0546141143983536,22.4546974637244,5.52884449237241));
#7862=CARTESIAN_POINT('Ctrl Pts',(0.02645207368245,22.46,5.53));
#7863=CARTESIAN_POINT('Ctrl Pts',(-0.02645207368245,22.46,5.53));
#7864=CARTESIAN_POINT('Ctrl Pts',(-0.0546141143983536,22.4546974637244,
5.52884449237241));
#7865=CARTESIAN_POINT('Ctrl Pts',(-0.102998643109697,22.434624043331,5.52493819304946));
#7866=CARTESIAN_POINT('Ctrl Pts',(-0.123818356698221,22.4212051523632,5.52245784982446));
#7867=CARTESIAN_POINT('Ctrl Pts',(-0.141067359796651,22.405563491861,5.52));
#7868=CARTESIAN_POINT('Origin',(0.,22.25,5.52));
#7869=CARTESIAN_POINT('',(-0.141067359796651,21.,5.52));
#7870=CARTESIAN_POINT('Origin',(-0.3,20.9,3.25));
#7871=CARTESIAN_POINT('',(-0.3,21.,3.25));
#7872=CARTESIAN_POINT('',(-0.3,21.,3.57606079858305));
#7873=CARTESIAN_POINT('',(-0.3,21.,3.89));
#7874=CARTESIAN_POINT('',(-0.3,23.5,3.25));
#7875=CARTESIAN_POINT('',(-0.3,20.9,3.25));
#7876=CARTESIAN_POINT('',(-0.3,23.5,3.57606079858305));
#7877=CARTESIAN_POINT('',(-0.3,23.5,3.89));
#7878=CARTESIAN_POINT('',(-0.3,21.,3.57606079858305));
#7879=CARTESIAN_POINT('Origin',(0.3,20.9,3.25));
#7880=CARTESIAN_POINT('',(0.3,21.,3.25));
#7881=CARTESIAN_POINT('',(0.15,21.,3.25));
#7882=CARTESIAN_POINT('',(0.3,23.5,3.25));
#7883=CARTESIAN_POINT('',(0.3,20.9,3.25));
#7884=CARTESIAN_POINT('',(0.15,23.5,3.25));
#7885=CARTESIAN_POINT('Origin',(0.3,20.9,4.53));
#7886=CARTESIAN_POINT('',(0.3,21.,3.57606079858305));
#7887=CARTESIAN_POINT('',(0.3,21.,4.53));
#7888=CARTESIAN_POINT('',(0.3,23.5,3.57606079858305));
#7889=CARTESIAN_POINT('',(0.3,21.,3.57606079858305));
#7890=CARTESIAN_POINT('',(0.3,23.5,4.53));
#7891=CARTESIAN_POINT('Origin',(0.,23.5,4.53));
#7892=CARTESIAN_POINT('',(-2.,23.5,4.53));
#7893=CARTESIAN_POINT('Origin',(0.,23.5,4.53));
#7894=CARTESIAN_POINT('Origin',(0.,23.5,4.53));
#7895=CARTESIAN_POINT('Origin',(0.,21.,4.53));
#7896=CARTESIAN_POINT('Origin',(0.,21.,4.53));
#7897=CARTESIAN_POINT('Origin',(0.,21.,4.53));
#7898=CARTESIAN_POINT('',(-2.,21.,4.53));
#7899=CARTESIAN_POINT('',(-2.,21.,4.53));
#7900=CARTESIAN_POINT('Origin',(0.,21.,4.53));
#7901=CARTESIAN_POINT('Origin',(0.,21.,4.53));
#7902=CARTESIAN_POINT('',(0.,0.,0.));
#7903=CARTESIAN_POINT('Origin',(0.,-1.25,5.52));
#7904=CARTESIAN_POINT('',(0.172988438920056,-1.36905880899792,5.52));
#7905=CARTESIAN_POINT('',(0.172988438920056,-1.13094119100209,5.52));
#7906=CARTESIAN_POINT('',(0.172988438920056,-1.65,5.52));
#7907=CARTESIAN_POINT('Origin',(0.,-1.25,5.52));
#7908=CARTESIAN_POINT('Origin',(0.,-1.25,5.52));
#7909=CARTESIAN_POINT('',(-0.172988438920056,-1.36905880899792,5.52));
#7910=CARTESIAN_POINT('Ctrl Pts',(-0.172988438920056,-1.36905880899792,
5.52));
#7911=CARTESIAN_POINT('Ctrl Pts',(-0.165594865311314,-1.37980142239529,
5.52129192197638));
#7912=CARTESIAN_POINT('Ctrl Pts',(-0.157297138725606,-1.38968770937274,
5.52265394943905));
#7913=CARTESIAN_POINT('Ctrl Pts',(-0.129892073845076,-1.41709277425327,
5.5267480843909));
#7914=CARTESIAN_POINT('Ctrl Pts',(-0.106330167759284,-1.43324205633295,
5.52969589327638));
#7915=CARTESIAN_POINT('Ctrl Pts',(-0.0546129046324105,-1.45469779396491,
5.53385029472357));
#7916=CARTESIAN_POINT('Ctrl Pts',(-0.0264512308298517,-1.46,5.535));
#7917=CARTESIAN_POINT('Ctrl Pts',(0.0264512308298516,-1.46,5.535));
#7918=CARTESIAN_POINT('Ctrl Pts',(0.0546129046324104,-1.45469779396491,
5.53385029472357));
#7919=CARTESIAN_POINT('Ctrl Pts',(0.106330167759284,-1.43324205633295,5.52969589327638));
#7920=CARTESIAN_POINT('Ctrl Pts',(0.129892073845076,-1.41709277425327,5.5267480843909));
#7921=CARTESIAN_POINT('Ctrl Pts',(0.157297138725606,-1.38968770937274,5.52265394943905));
#7922=CARTESIAN_POINT('Ctrl Pts',(0.165594865311314,-1.37980142239529,5.52129192197638));
#7923=CARTESIAN_POINT('Ctrl Pts',(0.172988438920056,-1.36905880899792,5.52));
#7924=CARTESIAN_POINT('',(-0.21,-1.25,5.52));
#7925=CARTESIAN_POINT('Origin',(0.,-1.25,5.52));
#7926=CARTESIAN_POINT('',(-0.21,-1.25,6.01522725533839));
#7927=CARTESIAN_POINT('',(-0.21,-1.25,5.52));
#7928=CARTESIAN_POINT('',(0.21,-1.25,6.01522725533839));
#7929=CARTESIAN_POINT('Ctrl Pts',(0.21,-1.25,6.01522725533839));
#7930=CARTESIAN_POINT('Ctrl Pts',(0.21,-1.27640552692445,6.01522725533839));
#7931=CARTESIAN_POINT('Ctrl Pts',(0.204715737269596,-1.30454707409071,6.01600415954412));
#7932=CARTESIAN_POINT('Ctrl Pts',(0.183273763036331,-1.35627626890513,6.01880073282317));
#7933=CARTESIAN_POINT('Ctrl Pts',(0.167117923970394,-1.37986692412796,6.02077897157582));
#7934=CARTESIAN_POINT('Ctrl Pts',(0.129867169887369,-1.41711767821098,6.02448481141327));
#7935=CARTESIAN_POINT('Ctrl Pts',(0.106276408305765,-1.43327371000135,6.02645455657129));
#7936=CARTESIAN_POINT('Ctrl Pts',(0.0545468514059002,-1.45471582482622,
6.02923165515645));
#7937=CARTESIAN_POINT('Ctrl Pts',(0.0264051785092814,-1.46,6.03));
#7938=CARTESIAN_POINT('Ctrl Pts',(-0.0264051785092814,-1.46,6.03));
#7939=CARTESIAN_POINT('Ctrl Pts',(-0.0545468514059001,-1.45471582482622,
6.02923165515645));
#7940=CARTESIAN_POINT('Ctrl Pts',(-0.106276408305765,-1.43327371000135,
6.02645455657129));
#7941=CARTESIAN_POINT('Ctrl Pts',(-0.129867169887369,-1.41711767821098,
6.02448481141327));
#7942=CARTESIAN_POINT('Ctrl Pts',(-0.167117923970394,-1.37986692412796,
6.02077897157582));
#7943=CARTESIAN_POINT('Ctrl Pts',(-0.183273763036331,-1.35627626890513,
6.01880073282317));
#7944=CARTESIAN_POINT('Ctrl Pts',(-0.204715737269596,-1.30454707409071,
6.01600415954412));
#7945=CARTESIAN_POINT('Ctrl Pts',(-0.21,-1.27640552692445,6.01522725533839));
#7946=CARTESIAN_POINT('Ctrl Pts',(-0.21,-1.25,6.01522725533839));
#7947=CARTESIAN_POINT('Ctrl Pts',(-0.21,-1.25,6.01522725533839));
#7948=CARTESIAN_POINT('Ctrl Pts',(-0.21,-1.22359447307555,6.01522725533839));
#7949=CARTESIAN_POINT('Ctrl Pts',(-0.204715737269596,-1.19545292590929,
6.01600415954412));
#7950=CARTESIAN_POINT('Ctrl Pts',(-0.183273763036331,-1.14372373109487,
6.01880073282317));
#7951=CARTESIAN_POINT('Ctrl Pts',(-0.167117923970394,-1.12013307587204,
6.02077897157582));
#7952=CARTESIAN_POINT('Ctrl Pts',(-0.129867169887369,-1.08288232178902,
6.02448481141327));
#7953=CARTESIAN_POINT('Ctrl Pts',(-0.106276408305765,-1.06672628999865,
6.02645455657129));
#7954=CARTESIAN_POINT('Ctrl Pts',(-0.0545468514059002,-1.04528417517378,
6.02923165515645));
#7955=CARTESIAN_POINT('Ctrl Pts',(-0.0264051785092814,-1.04,6.03));
#7956=CARTESIAN_POINT('Ctrl Pts',(0.0264051785092814,-1.04,6.03));
#7957=CARTESIAN_POINT('Ctrl Pts',(0.0545468514059001,-1.04528417517378,
6.02923165515645));
#7958=CARTESIAN_POINT('Ctrl Pts',(0.106276408305765,-1.06672628999865,6.02645455657129));
#7959=CARTESIAN_POINT('Ctrl Pts',(0.129867169887369,-1.08288232178902,6.02448481141327));
#7960=CARTESIAN_POINT('Ctrl Pts',(0.167117923970394,-1.12013307587204,6.02077897157582));
#7961=CARTESIAN_POINT('Ctrl Pts',(0.183273763036331,-1.14372373109487,6.01880073282317));
#7962=CARTESIAN_POINT('Ctrl Pts',(0.204715737269596,-1.19545292590929,6.01600415954412));
#7963=CARTESIAN_POINT('Ctrl Pts',(0.21,-1.22359447307555,6.01522725533839));
#7964=CARTESIAN_POINT('Ctrl Pts',(0.21,-1.25,6.01522725533839));
#7965=CARTESIAN_POINT('',(-0.172988438920056,-1.13094119100209,5.52));
#7966=CARTESIAN_POINT('Origin',(0.,-1.25,5.52));
#7967=CARTESIAN_POINT('Ctrl Pts',(0.172988438920056,-1.13094119100209,5.52));
#7968=CARTESIAN_POINT('Ctrl Pts',(0.165594865311315,-1.12019857760471,5.52129192197638));
#7969=CARTESIAN_POINT('Ctrl Pts',(0.157297138725606,-1.11031229062726,5.52265394943905));
#7970=CARTESIAN_POINT('Ctrl Pts',(0.129892073845076,-1.08290722574673,5.5267480843909));
#7971=CARTESIAN_POINT('Ctrl Pts',(0.106330167759284,-1.06675794366705,5.52969589327638));
#7972=CARTESIAN_POINT('Ctrl Pts',(0.0546129046324104,-1.04530220603509,
5.53385029472357));
#7973=CARTESIAN_POINT('Ctrl Pts',(0.0264512308298516,-1.04,5.535));
#7974=CARTESIAN_POINT('Ctrl Pts',(-0.0264512308298516,-1.04,5.535));
#7975=CARTESIAN_POINT('Ctrl Pts',(-0.0546129046324104,-1.04530220603509,
5.53385029472357));
#7976=CARTESIAN_POINT('Ctrl Pts',(-0.106330167759284,-1.06675794366705,
5.52969589327638));
#7977=CARTESIAN_POINT('Ctrl Pts',(-0.129892073845076,-1.08290722574673,
5.5267480843909));
#7978=CARTESIAN_POINT('Ctrl Pts',(-0.157297138725606,-1.11031229062726,
5.52265394943905));
#7979=CARTESIAN_POINT('Ctrl Pts',(-0.165594865311315,-1.12019857760471,
5.52129192197638));
#7980=CARTESIAN_POINT('Ctrl Pts',(-0.172988438920056,-1.13094119100209,
5.52));
#7981=CARTESIAN_POINT('Origin',(0.,-1.25,5.52));
#7982=CARTESIAN_POINT('',(-0.172988438920056,-1.65,5.52));
#7983=CARTESIAN_POINT('Origin',(0.,-1.65,4.53));
#7984=CARTESIAN_POINT('',(-1.005,-0.85,4.53));
#7985=CARTESIAN_POINT('Origin',(0.,-0.85,4.53));
#7986=CARTESIAN_POINT('',(-1.005,-1.65,4.53));
#7987=CARTESIAN_POINT('',(-1.005,-1.65,4.53));
#7988=CARTESIAN_POINT('Origin',(0.,-1.65,4.53));
#7989=CARTESIAN_POINT('Origin',(0.,-1.65,4.53));
#7990=CARTESIAN_POINT('',(-1.5,-0.85,4.53));
#7991=CARTESIAN_POINT('Origin',(0.,-0.85,4.53));
#7992=CARTESIAN_POINT('',(-1.5,-1.65,4.53));
#7993=CARTESIAN_POINT('',(-1.5,-1.65,4.53));
#7994=CARTESIAN_POINT('Origin',(0.,-1.65,4.53));
#7995=CARTESIAN_POINT('Origin',(0.,-0.85,4.53));
#7996=CARTESIAN_POINT('Origin',(0.,-1.65,4.53));
#7997=CARTESIAN_POINT('',(0.,0.,0.));
#7998=CARTESIAN_POINT('Origin',(0.,32.85,5.52));
#7999=CARTESIAN_POINT('',(0.172988438920056,32.7309411910021,5.52));
#8000=CARTESIAN_POINT('',(0.172988438920056,32.9690588089979,5.52));
#8001=CARTESIAN_POINT('',(0.172988438920056,32.45,5.52));
#8002=CARTESIAN_POINT('Origin',(0.,32.85,5.52));
#8003=CARTESIAN_POINT('Origin',(0.,32.85,5.52));
#8004=CARTESIAN_POINT('',(-0.172988438920056,32.7309411910021,5.52));
#8005=CARTESIAN_POINT('Ctrl Pts',(-0.172988438920059,32.7309411910021,5.52));
#8006=CARTESIAN_POINT('Ctrl Pts',(-0.165594865311318,32.7201985776047,5.52129192197638));
#8007=CARTESIAN_POINT('Ctrl Pts',(-0.157297138725607,32.7103122906273,5.52265394943905));
#8008=CARTESIAN_POINT('Ctrl Pts',(-0.129892073845076,32.6829072257467,5.5267480843909));
#8009=CARTESIAN_POINT('Ctrl Pts',(-0.106330167759285,32.6667579436671,5.52969589327637));
#8010=CARTESIAN_POINT('Ctrl Pts',(-0.0546129046324106,32.6453022060351,
5.53385029472357));
#8011=CARTESIAN_POINT('Ctrl Pts',(-0.0264512308298518,32.64,5.535));
#8012=CARTESIAN_POINT('Ctrl Pts',(0.0264512308298517,32.64,5.535));
#8013=CARTESIAN_POINT('Ctrl Pts',(0.0546129046324105,32.6453022060351,5.53385029472357));
#8014=CARTESIAN_POINT('Ctrl Pts',(0.106330167759285,32.6667579436671,5.52969589327637));
#8015=CARTESIAN_POINT('Ctrl Pts',(0.129892073845076,32.6829072257467,5.5267480843909));
#8016=CARTESIAN_POINT('Ctrl Pts',(0.157297138725608,32.7103122906273,5.52265394943905));
#8017=CARTESIAN_POINT('Ctrl Pts',(0.165594865311314,32.7201985776047,5.52129192197638));
#8018=CARTESIAN_POINT('Ctrl Pts',(0.172988438920054,32.7309411910021,5.52));
#8019=CARTESIAN_POINT('',(-0.21,32.85,5.52));
#8020=CARTESIAN_POINT('Origin',(0.,32.85,5.52));
#8021=CARTESIAN_POINT('',(-0.21,32.85,6.01522725533839));
#8022=CARTESIAN_POINT('',(-0.21,32.85,5.52));
#8023=CARTESIAN_POINT('',(0.21,32.85,6.01522725533839));
#8024=CARTESIAN_POINT('Ctrl Pts',(0.21,32.85,6.01522725533839));
#8025=CARTESIAN_POINT('Ctrl Pts',(0.21,32.8235944730755,6.01522725533839));
#8026=CARTESIAN_POINT('Ctrl Pts',(0.204715737269596,32.7954529259093,6.01600415954412));
#8027=CARTESIAN_POINT('Ctrl Pts',(0.183273763036331,32.7437237310949,6.01880073282317));
#8028=CARTESIAN_POINT('Ctrl Pts',(0.167117923970393,32.720133075872,6.02077897157582));
#8029=CARTESIAN_POINT('Ctrl Pts',(0.129867169887369,32.682882321789,6.02448481141327));
#8030=CARTESIAN_POINT('Ctrl Pts',(0.106276408305765,32.6667262899986,6.02645455657129));
#8031=CARTESIAN_POINT('Ctrl Pts',(0.0545468514058989,32.6452841751738,6.02923165515645));
#8032=CARTESIAN_POINT('Ctrl Pts',(0.0264051785092816,32.64,6.03));
#8033=CARTESIAN_POINT('Ctrl Pts',(-0.0264051785092815,32.64,6.03));
#8034=CARTESIAN_POINT('Ctrl Pts',(-0.0545468514058988,32.6452841751738,
6.02923165515645));
#8035=CARTESIAN_POINT('Ctrl Pts',(-0.106276408305765,32.6667262899986,6.02645455657129));
#8036=CARTESIAN_POINT('Ctrl Pts',(-0.129867169887368,32.682882321789,6.02448481141327));
#8037=CARTESIAN_POINT('Ctrl Pts',(-0.167117923970393,32.720133075872,6.02077897157582));
#8038=CARTESIAN_POINT('Ctrl Pts',(-0.183273763036331,32.7437237310949,6.01880073282317));
#8039=CARTESIAN_POINT('Ctrl Pts',(-0.204715737269596,32.7954529259093,6.01600415954412));
#8040=CARTESIAN_POINT('Ctrl Pts',(-0.210000000000001,32.8235944730755,6.01522725533839));
#8041=CARTESIAN_POINT('Ctrl Pts',(-0.210000000000001,32.85,6.01522725533839));
#8042=CARTESIAN_POINT('Ctrl Pts',(-0.21,32.85,6.01522725533839));
#8043=CARTESIAN_POINT('Ctrl Pts',(-0.21,32.8764055269245,6.01522725533839));
#8044=CARTESIAN_POINT('Ctrl Pts',(-0.204715737269596,32.9045470740907,6.01600415954412));
#8045=CARTESIAN_POINT('Ctrl Pts',(-0.183273763036331,32.9562762689051,6.01880073282317));
#8046=CARTESIAN_POINT('Ctrl Pts',(-0.167117923970393,32.979866924128,6.02077897157582));
#8047=CARTESIAN_POINT('Ctrl Pts',(-0.129867169887369,33.017117678211,6.02448481141327));
#8048=CARTESIAN_POINT('Ctrl Pts',(-0.106276408305765,33.0332737100014,6.02645455657129));
#8049=CARTESIAN_POINT('Ctrl Pts',(-0.0545468514058989,33.0547158248262,
6.02923165515645));
#8050=CARTESIAN_POINT('Ctrl Pts',(-0.0264051785092816,33.06,6.03));
#8051=CARTESIAN_POINT('Ctrl Pts',(0.0264051785092815,33.06,6.03));
#8052=CARTESIAN_POINT('Ctrl Pts',(0.0545468514058988,33.0547158248262,6.02923165515645));
#8053=CARTESIAN_POINT('Ctrl Pts',(0.106276408305765,33.0332737100014,6.02645455657129));
#8054=CARTESIAN_POINT('Ctrl Pts',(0.129867169887368,33.017117678211,6.02448481141327));
#8055=CARTESIAN_POINT('Ctrl Pts',(0.167117923970393,32.979866924128,6.02077897157582));
#8056=CARTESIAN_POINT('Ctrl Pts',(0.183273763036331,32.9562762689051,6.01880073282317));
#8057=CARTESIAN_POINT('Ctrl Pts',(0.204715737269596,32.9045470740907,6.01600415954412));
#8058=CARTESIAN_POINT('Ctrl Pts',(0.21,32.8764055269245,6.01522725533839));
#8059=CARTESIAN_POINT('Ctrl Pts',(0.21,32.85,6.01522725533839));
#8060=CARTESIAN_POINT('',(-0.172988438920056,32.9690588089979,5.52));
#8061=CARTESIAN_POINT('Origin',(0.,32.85,5.52));
#8062=CARTESIAN_POINT('Ctrl Pts',(0.172988438920058,32.9690588089979,5.52));
#8063=CARTESIAN_POINT('Ctrl Pts',(0.165594865311317,32.9798014223953,5.52129192197638));
#8064=CARTESIAN_POINT('Ctrl Pts',(0.157297138725607,32.9896877093727,5.52265394943905));
#8065=CARTESIAN_POINT('Ctrl Pts',(0.129892073845076,33.0170927742533,5.5267480843909));
#8066=CARTESIAN_POINT('Ctrl Pts',(0.106330167759285,33.033242056333,5.52969589327637));
#8067=CARTESIAN_POINT('Ctrl Pts',(0.0546129046324106,33.0546977939649,5.53385029472357));
#8068=CARTESIAN_POINT('Ctrl Pts',(0.0264512308298518,33.06,5.535));
#8069=CARTESIAN_POINT('Ctrl Pts',(-0.0264512308298517,33.06,5.535));
#8070=CARTESIAN_POINT('Ctrl Pts',(-0.0546129046324106,33.0546977939649,
5.53385029472357));
#8071=CARTESIAN_POINT('Ctrl Pts',(-0.106330167759285,33.033242056333,5.52969589327637));
#8072=CARTESIAN_POINT('Ctrl Pts',(-0.129892073845076,33.0170927742533,5.5267480843909));
#8073=CARTESIAN_POINT('Ctrl Pts',(-0.157297138725607,32.9896877093727,5.52265394943905));
#8074=CARTESIAN_POINT('Ctrl Pts',(-0.165594865311317,32.9798014223953,5.52129192197638));
#8075=CARTESIAN_POINT('Ctrl Pts',(-0.172988438920057,32.9690588089979,5.52));
#8076=CARTESIAN_POINT('Origin',(0.,32.85,5.52));
#8077=CARTESIAN_POINT('',(-0.172988438920056,32.45,5.52));
#8078=CARTESIAN_POINT('Origin',(0.,32.45,4.53));
#8079=CARTESIAN_POINT('',(-1.005,33.25,4.53));
#8080=CARTESIAN_POINT('Origin',(0.,33.25,4.53));
#8081=CARTESIAN_POINT('',(-1.005,32.45,4.53));
#8082=CARTESIAN_POINT('',(-1.005,32.45,4.53));
#8083=CARTESIAN_POINT('Origin',(0.,32.45,4.53));
#8084=CARTESIAN_POINT('Origin',(0.,32.45,4.53));
#8085=CARTESIAN_POINT('',(-1.5,33.25,4.53));
#8086=CARTESIAN_POINT('Origin',(0.,33.25,4.53));
#8087=CARTESIAN_POINT('',(-1.5,32.45,4.53));
#8088=CARTESIAN_POINT('',(-1.5,32.45,4.53));
#8089=CARTESIAN_POINT('Origin',(0.,32.45,4.53));
#8090=CARTESIAN_POINT('Origin',(0.,33.25,4.53));
#8091=CARTESIAN_POINT('Origin',(0.,32.45,4.53));
#8092=CARTESIAN_POINT('',(0.,0.,0.));
#8093=CARTESIAN_POINT('Origin',(0.,-4.7,4.53));
#8094=CARTESIAN_POINT('',(-0.275,-4.5,4.53));
#8095=CARTESIAN_POINT('Origin',(0.,-4.5,4.53));
#8096=CARTESIAN_POINT('',(-0.275,-4.7,4.53));
#8097=CARTESIAN_POINT('',(-0.275,-4.7,4.53));
#8098=CARTESIAN_POINT('Origin',(0.,-4.7,4.53));
#8099=CARTESIAN_POINT('Origin',(0.,-4.7,4.53));
#8100=CARTESIAN_POINT('',(-1.1,-4.5,4.53));
#8101=CARTESIAN_POINT('Origin',(0.,-4.5,4.53));
#8102=CARTESIAN_POINT('',(-1.1,-4.7,4.53));
#8103=CARTESIAN_POINT('',(-1.1,-4.7,4.53));
#8104=CARTESIAN_POINT('Origin',(0.,-4.7,4.53));
#8105=CARTESIAN_POINT('Origin',(0.,-4.5,4.53));
#8106=CARTESIAN_POINT('Origin',(0.,-4.7,4.53));
#8107=CARTESIAN_POINT('',(0.,0.,0.));
#8108=CARTESIAN_POINT('Origin',(0.,34.5,4.53));
#8109=CARTESIAN_POINT('',(-0.275,34.7,4.53));
#8110=CARTESIAN_POINT('Origin',(0.,34.7,4.53));
#8111=CARTESIAN_POINT('',(-0.275,34.5,4.53));
#8112=CARTESIAN_POINT('',(-0.275,34.5,4.53));
#8113=CARTESIAN_POINT('Origin',(0.,34.5,4.53));
#8114=CARTESIAN_POINT('Origin',(0.,34.5,4.53));
#8115=CARTESIAN_POINT('',(-1.1,34.7,4.53));
#8116=CARTESIAN_POINT('Origin',(0.,34.7,4.53));
#8117=CARTESIAN_POINT('',(-1.1,34.5,4.53));
#8118=CARTESIAN_POINT('',(-1.1,34.5,4.53));
#8119=CARTESIAN_POINT('Origin',(0.,34.5,4.53));
#8120=CARTESIAN_POINT('Origin',(0.,34.7,4.53));
#8121=CARTESIAN_POINT('Origin',(0.,34.5,4.53));
#8122=CARTESIAN_POINT('',(0.,0.,0.));
#8123=CARTESIAN_POINT('Origin',(-1.,0.,0.35));
#8124=CARTESIAN_POINT('',(-1.,-0.26,0.6));
#8125=CARTESIAN_POINT('',(-1.,-0.3,0.56));
#8126=CARTESIAN_POINT('',(-1.,-0.2675,0.5925));
#8127=CARTESIAN_POINT('',(-1.,0.26,0.6));
#8128=CARTESIAN_POINT('',(-1.,0.,0.6));
#8129=CARTESIAN_POINT('',(-1.,0.3,0.56));
#8130=CARTESIAN_POINT('',(-1.,0.2675,0.5925));
#8131=CARTESIAN_POINT('',(-1.,0.3,0.04));
#8132=CARTESIAN_POINT('',(-1.,0.3,0.175));
#8133=CARTESIAN_POINT('',(-1.,0.26,0.));
#8134=CARTESIAN_POINT('',(-1.,0.2925,0.0325));
#8135=CARTESIAN_POINT('',(-1.,-0.26,0.));
#8136=CARTESIAN_POINT('',(-1.,0.,0.));
#8137=CARTESIAN_POINT('',(-1.,-0.3,0.04));
#8138=CARTESIAN_POINT('',(-1.,-0.2925,0.0325));
#8139=CARTESIAN_POINT('',(-1.,-0.3,0.175));
#8140=CARTESIAN_POINT('Origin',(0.75,0.28,0.02));
#8141=CARTESIAN_POINT('',(1.,0.3,0.04));
#8142=CARTESIAN_POINT('',(0.75,0.3,0.04));
#8143=CARTESIAN_POINT('',(1.,0.26,0.));
#8144=CARTESIAN_POINT('',(1.,0.2925,0.0325));
#8145=CARTESIAN_POINT('',(0.75,0.26,0.));
#8146=CARTESIAN_POINT('Origin',(1.5,0.3,0.));
#8147=CARTESIAN_POINT('',(1.,0.3,0.56));
#8148=CARTESIAN_POINT('',(0.75,0.3,0.56));
#8149=CARTESIAN_POINT('',(1.,0.3,0.175));
#8150=CARTESIAN_POINT('Origin',(0.75,0.28,0.58));
#8151=CARTESIAN_POINT('',(1.,0.26,0.6));
#8152=CARTESIAN_POINT('',(0.75,0.26,0.6));
#8153=CARTESIAN_POINT('',(1.,0.2675,0.5925));
#8154=CARTESIAN_POINT('Origin',(0.,0.,0.6));
#8155=CARTESIAN_POINT('',(1.,-0.26,0.6));
#8156=CARTESIAN_POINT('',(-0.75,-0.26,0.6));
#8157=CARTESIAN_POINT('',(1.,0.,0.6));
#8158=CARTESIAN_POINT('Origin',(1.,0.,0.35));
#8159=CARTESIAN_POINT('',(1.,-0.26,0.));
#8160=CARTESIAN_POINT('',(1.,-0.3,0.04));
#8161=CARTESIAN_POINT('',(1.,-0.2925,0.0325));
#8162=CARTESIAN_POINT('',(1.,0.,0.));
#8163=CARTESIAN_POINT('',(1.,-0.3,0.56));
#8164=CARTESIAN_POINT('',(1.,-0.2675,0.5925));
#8165=CARTESIAN_POINT('',(1.,-0.3,0.175));
#8166=CARTESIAN_POINT('Origin',(0.,0.,0.));
#8167=CARTESIAN_POINT('',(-0.75,-0.26,0.));
#8168=CARTESIAN_POINT('Origin',(-0.75,-0.28,0.58));
#8169=CARTESIAN_POINT('',(-0.75,-0.3,0.56));
#8170=CARTESIAN_POINT('Origin',(-0.75,-0.28,0.02));
#8171=CARTESIAN_POINT('',(-0.75,-0.3,0.04));
#8172=CARTESIAN_POINT('Origin',(-1.5,-0.3,0.));
#8173=CARTESIAN_POINT('',(0.,0.,0.));
#8174=CARTESIAN_POINT('Origin',(0.0721687836487032,0.,-0.125));
#8175=CARTESIAN_POINT('',(0.0721687836487032,0.,-0.125));
#8176=CARTESIAN_POINT('',(0.144337567297406,0.,0.));
#8177=CARTESIAN_POINT('',(0.117710979560879,0.,-0.0461186027918559));
#8178=CARTESIAN_POINT('',(0.0721687836487032,-0.25,-0.125));
#8179=CARTESIAN_POINT('',(0.0721687836487032,0.,-0.125));
#8180=CARTESIAN_POINT('',(0.144337567297406,-0.25,0.));
#8181=CARTESIAN_POINT('',(0.144337567297406,-0.25,0.));
#8182=CARTESIAN_POINT('',(0.144337567297406,0.,0.));
#8183=CARTESIAN_POINT('Origin',(-0.0721687836487032,0.,-0.125));
#8184=CARTESIAN_POINT('',(-0.0721687836487032,0.,-0.125));
#8185=CARTESIAN_POINT('',(0.0739156081756484,0.,-0.125));
#8186=CARTESIAN_POINT('',(-0.0721687836487032,-0.25,-0.125));
#8187=CARTESIAN_POINT('',(-0.0721687836487032,0.,-0.125));
#8188=CARTESIAN_POINT('',(0.0721687836487032,-0.25,-0.125));
#8189=CARTESIAN_POINT('Origin',(-0.144337567297406,0.,-4.16333634234434E-17));
#8190=CARTESIAN_POINT('',(-0.144337567297406,0.,-1.76762539787485E-17));
#8191=CARTESIAN_POINT('',(-0.0987953713852306,0.,-0.0788813972081442));
#8192=CARTESIAN_POINT('',(-0.144337567297406,-0.25,-2.77555756156289E-17));
#8193=CARTESIAN_POINT('',(-0.144337567297406,0.,-1.76762539787485E-17));
#8194=CARTESIAN_POINT('',(-0.0721687836487032,-0.25,-0.125));
#8195=CARTESIAN_POINT('Origin',(-0.0721687836487033,0.,0.125));
#8196=CARTESIAN_POINT('',(-0.0721687836487033,0.,0.125));
#8197=CARTESIAN_POINT('',(-0.0627109795608791,0.,0.141381397208144));
#8198=CARTESIAN_POINT('',(-0.0721687836487033,-0.25,0.125));
#8199=CARTESIAN_POINT('',(-0.0721687836487033,0.,0.125));
#8200=CARTESIAN_POINT('',(-0.144337567297406,-0.25,-1.76762539787485E-17));
#8201=CARTESIAN_POINT('Origin',(0.0721687836487032,0.,0.125));
#8202=CARTESIAN_POINT('',(0.0721687836487032,0.,0.125));
#8203=CARTESIAN_POINT('',(0.146084391824352,0.,0.125));
#8204=CARTESIAN_POINT('',(0.0721687836487032,-0.25,0.125));
#8205=CARTESIAN_POINT('',(0.0721687836487032,0.,0.125));
#8206=CARTESIAN_POINT('',(-0.0721687836487033,-0.25,0.125));
#8207=CARTESIAN_POINT('Origin',(0.144337567297406,0.,0.));
#8208=CARTESIAN_POINT('',(0.153795371385231,0.,-0.0163813972081441));
#8209=CARTESIAN_POINT('',(0.0721687836487032,-0.25,0.125));
#8210=CARTESIAN_POINT('Origin',(0.,-0.25,0.));
#8211=CARTESIAN_POINT('Origin',(0.22,0.,0.));
#8212=CARTESIAN_POINT('',(-0.22,-8.67361737988404E-18,-2.69422295812418E-17));
#8213=CARTESIAN_POINT('Origin',(0.,0.,0.));
#8214=CARTESIAN_POINT('Origin',(0.,-0.015,0.));
#8215=CARTESIAN_POINT('',(-0.24505,-0.02505,-3.00099698131059E-17));
#8216=CARTESIAN_POINT('Origin',(0.,-0.02505,0.));
#8217=CARTESIAN_POINT('',(-0.235,-0.015,-2.87791997799628E-17));
#8218=CARTESIAN_POINT('Origin',(0.,-0.3775,0.));
#8219=CARTESIAN_POINT('',(-0.24505,-0.72995,3.00099698131059E-17));
#8220=CARTESIAN_POINT('Origin',(0.,-0.72995,0.));
#8221=CARTESIAN_POINT('',(-0.24505,-0.3775,-3.00099698131059E-17));
#8222=CARTESIAN_POINT('Origin',(0.,-0.7625,0.));
#8223=CARTESIAN_POINT('',(-0.175,-0.8,-2.14313189850787E-17));
#8224=CARTESIAN_POINT('Origin',(0.,-0.8,0.));
#8225=CARTESIAN_POINT('',(-0.2125,-0.7625,-2.60237444818813E-17));
#8226=CARTESIAN_POINT('Origin',(0.,-0.8,0.));
#8227=CARTESIAN_POINT('',(0.,0.,0.));
#8228=CARTESIAN_POINT('Origin',(0.375,0.5,0.));
#8229=CARTESIAN_POINT('',(-0.375,0.5,-4.59242549680257E-17));
#8230=CARTESIAN_POINT('Origin',(0.,0.5,0.));
#8231=CARTESIAN_POINT('Origin',(0.,0.475,0.));
#8232=CARTESIAN_POINT('',(-0.425,0.45,-5.20474889637625E-17));
#8233=CARTESIAN_POINT('Origin',(0.,0.45,0.));
#8234=CARTESIAN_POINT('',(-0.4,0.475,-4.89858719658941E-17));
#8235=CARTESIAN_POINT('Origin',(0.,0.24,0.));
#8236=CARTESIAN_POINT('',(-0.425,0.0299999999999998,-5.20474889637625E-17));
#8237=CARTESIAN_POINT('Origin',(0.,0.0299999999999998,0.));
#8238=CARTESIAN_POINT('',(-0.425,0.24,-5.20474889637625E-17));
#8239=CARTESIAN_POINT('Origin',(0.,0.0150000000000001,0.));
#8240=CARTESIAN_POINT('',(-0.395,4.85722573273506E-17,-4.83735485663204E-17));
#8241=CARTESIAN_POINT('Origin',(0.,0.,0.));
#8242=CARTESIAN_POINT('',(-0.41,0.0150000000000001,-5.02105187650415E-17));
#8243=CARTESIAN_POINT('Origin',(0.27,0.,0.));
#8244=CARTESIAN_POINT('',(-0.27,0.,-3.30654635769785E-17));
#8245=CARTESIAN_POINT('Origin',(0.,0.,0.));
#8246=CARTESIAN_POINT('Origin',(0.,-0.02,0.));
#8247=CARTESIAN_POINT('',(-0.24505,-0.0498999999999999,3.00099698131059E-17));
#8248=CARTESIAN_POINT('Origin',(0.,-0.0498999999999999,0.));
#8249=CARTESIAN_POINT('',(-0.26,-0.02,-3.18408167778312E-17));
#8250=CARTESIAN_POINT('Origin',(0.,-0.995,0.));
#8251=CARTESIAN_POINT('',(-0.24505,-1.95495,3.00099698131059E-17));
#8252=CARTESIAN_POINT('Origin',(0.,-1.95495,0.));
#8253=CARTESIAN_POINT('',(-0.24505,-0.995,-3.00099698131059E-17));
#8254=CARTESIAN_POINT('Origin',(0.,-1.975,0.));
#8255=CARTESIAN_POINT('',(-0.2,-2.,-2.44929359829471E-17));
#8256=CARTESIAN_POINT('Origin',(0.,-2.,0.));
#8257=CARTESIAN_POINT('',(-0.225,-1.975,-2.75545529808154E-17));
#8258=CARTESIAN_POINT('Origin',(0.,-2.,0.));
#8259=CARTESIAN_POINT('Origin',(0.115470053837925,-0.5,-0.2));
#8260=CARTESIAN_POINT('',(0.23094010767585,-0.5,0.));
#8261=CARTESIAN_POINT('',(0.115470053837925,-0.5,-0.2));
#8262=CARTESIAN_POINT('',(0.23094010767585,-0.5,0.));
#8263=CARTESIAN_POINT('',(0.115470053837925,-0.8,-0.2));
#8264=CARTESIAN_POINT('',(0.115470053837925,-0.5,-0.2));
#8265=CARTESIAN_POINT('',(0.23094010767585,-0.8,0.));
#8266=CARTESIAN_POINT('',(0.23094010767585,-0.8,0.));
#8267=CARTESIAN_POINT('',(0.23094010767585,-0.5,0.));
#8268=CARTESIAN_POINT('Origin',(-0.115470053837925,-0.5,-0.2));
#8269=CARTESIAN_POINT('',(-0.115470053837925,-0.5,-0.2));
#8270=CARTESIAN_POINT('',(0.115470053837925,-0.5,-0.2));
#8271=CARTESIAN_POINT('',(-0.115470053837925,-0.8,-0.2));
#8272=CARTESIAN_POINT('',(-0.115470053837925,-0.5,-0.2));
#8273=CARTESIAN_POINT('',(0.115470053837925,-0.8,-0.2));
#8274=CARTESIAN_POINT('Origin',(-0.23094010767585,-0.5,-2.77555756156289E-17));
#8275=CARTESIAN_POINT('',(-0.23094010767585,-0.5,-2.82820063659975E-17));
#8276=CARTESIAN_POINT('',(-0.115470053837925,-0.5,-0.2));
#8277=CARTESIAN_POINT('',(-0.23094010767585,-0.8,-2.77555756156289E-17));
#8278=CARTESIAN_POINT('',(-0.23094010767585,-0.5,-2.82820063659975E-17));
#8279=CARTESIAN_POINT('',(-0.115470053837925,-0.8,-0.2));
#8280=CARTESIAN_POINT('Origin',(-0.115470053837925,-0.5,0.2));
#8281=CARTESIAN_POINT('',(-0.115470053837925,-0.5,0.2));
#8282=CARTESIAN_POINT('',(-0.23094010767585,-0.5,-2.82820063659975E-17));
#8283=CARTESIAN_POINT('',(-0.115470053837925,-0.8,0.2));
#8284=CARTESIAN_POINT('',(-0.115470053837925,-0.5,0.2));
#8285=CARTESIAN_POINT('',(-0.23094010767585,-0.8,-2.82820063659975E-17));
#8286=CARTESIAN_POINT('Origin',(0.115470053837925,-0.5,0.2));
#8287=CARTESIAN_POINT('',(0.115470053837925,-0.5,0.2));
#8288=CARTESIAN_POINT('',(-0.115470053837925,-0.5,0.2));
#8289=CARTESIAN_POINT('',(0.115470053837925,-0.8,0.2));
#8290=CARTESIAN_POINT('',(0.115470053837925,-0.5,0.2));
#8291=CARTESIAN_POINT('',(-0.115470053837925,-0.8,0.2));
#8292=CARTESIAN_POINT('Origin',(0.23094010767585,-0.5,0.));
#8293=CARTESIAN_POINT('',(0.115470053837925,-0.5,0.2));
#8294=CARTESIAN_POINT('',(0.115470053837925,-0.8,0.2));
#8295=CARTESIAN_POINT('Origin',(0.,-0.5,0.));
#8296=CARTESIAN_POINT('Origin',(0.,-0.8,0.));
#8297=CARTESIAN_POINT('',(0.,0.,0.));
#8298=CARTESIAN_POINT('',(0.,0.,0.));
#8299=CARTESIAN_POINT('',(0.,0.,0.));
#8300=CARTESIAN_POINT('',(0.,0.,0.));
#8301=CARTESIAN_POINT('',(0.,0.,0.));
#8302=CARTESIAN_POINT('',(0.,0.,0.));
#8303=CARTESIAN_POINT('',(0.,0.,0.));
#8304=CARTESIAN_POINT('',(0.,7.25,3.88));
#8305=CARTESIAN_POINT('',(0.,7.25,6.33));
#8306=CARTESIAN_POINT('',(-9.04229427454561E-31,22.25,3.88));
#8307=CARTESIAN_POINT('',(0.,22.25,6.33));
#8308=CARTESIAN_POINT('',(0.,-1.25,6.33));
#8309=CARTESIAN_POINT('',(0.,32.85,6.33));
#8310=CARTESIAN_POINT('',(0.,-4.7,4.53));
#8311=CARTESIAN_POINT('',(0.,34.7,4.53));
#8312=CARTESIAN_POINT('',(0.,0.,0.));
#8313=CARTESIAN_POINT('',(0.,0.,0.));
#8314=UNCERTAINTY_MEASURE_WITH_UNIT(LENGTH_MEASURE(0.001),#8378,
'DISTANCE_ACCURACY_VALUE',
'Maximum model space distance between geometric entities at asserted c
onnectivities');
#8315=UNCERTAINTY_MEASURE_WITH_UNIT(LENGTH_MEASURE(0.001),#8378,
'DISTANCE_ACCURACY_VALUE',
'Maximum model space distance between geometric entities at asserted c
onnectivities');
#8316=UNCERTAINTY_MEASURE_WITH_UNIT(LENGTH_MEASURE(0.001),#8378,
'DISTANCE_ACCURACY_VALUE',
'Maximum model space distance between geometric entities at asserted c
onnectivities');
#8317=UNCERTAINTY_MEASURE_WITH_UNIT(LENGTH_MEASURE(0.001),#8378,
'DISTANCE_ACCURACY_VALUE',
'Maximum model space distance between geometric entities at asserted c
onnectivities');
#8318=UNCERTAINTY_MEASURE_WITH_UNIT(LENGTH_MEASURE(0.001),#8378,
'DISTANCE_ACCURACY_VALUE',
'Maximum model space distance between geometric entities at asserted c
onnectivities');
#8319=UNCERTAINTY_MEASURE_WITH_UNIT(LENGTH_MEASURE(0.001),#8378,
'DISTANCE_ACCURACY_VALUE',
'Maximum model space distance between geometric entities at asserted c
onnectivities');
#8320=UNCERTAINTY_MEASURE_WITH_UNIT(LENGTH_MEASURE(0.001),#8378,
'DISTANCE_ACCURACY_VALUE',
'Maximum model space distance between geometric entities at asserted c
onnectivities');
#8321=UNCERTAINTY_MEASURE_WITH_UNIT(LENGTH_MEASURE(0.001),#8378,
'DISTANCE_ACCURACY_VALUE',
'Maximum model space distance between geometric entities at asserted c
onnectivities');
#8322=UNCERTAINTY_MEASURE_WITH_UNIT(LENGTH_MEASURE(0.001),#8378,
'DISTANCE_ACCURACY_VALUE',
'Maximum model space distance between geometric entities at asserted c
onnectivities');
#8323=UNCERTAINTY_MEASURE_WITH_UNIT(LENGTH_MEASURE(0.001),#8378,
'DISTANCE_ACCURACY_VALUE',
'Maximum model space distance between geometric entities at asserted c
onnectivities');
#8324=UNCERTAINTY_MEASURE_WITH_UNIT(LENGTH_MEASURE(0.001),#8378,
'DISTANCE_ACCURACY_VALUE',
'Maximum model space distance between geometric entities at asserted c
onnectivities');
#8325=UNCERTAINTY_MEASURE_WITH_UNIT(LENGTH_MEASURE(0.001),#8378,
'DISTANCE_ACCURACY_VALUE',
'Maximum model space distance between geometric entities at asserted c
onnectivities');
#8326=UNCERTAINTY_MEASURE_WITH_UNIT(LENGTH_MEASURE(0.001),#8378,
'DISTANCE_ACCURACY_VALUE',
'Maximum model space distance between geometric entities at asserted c
onnectivities');
#8327=UNCERTAINTY_MEASURE_WITH_UNIT(LENGTH_MEASURE(0.001),#8378,
'DISTANCE_ACCURACY_VALUE',
'Maximum model space distance between geometric entities at asserted c
onnectivities');
#8328=UNCERTAINTY_MEASURE_WITH_UNIT(LENGTH_MEASURE(0.001),#8378,
'DISTANCE_ACCURACY_VALUE',
'Maximum model space distance between geometric entities at asserted c
onnectivities');
#8329=UNCERTAINTY_MEASURE_WITH_UNIT(LENGTH_MEASURE(0.001),#8378,
'DISTANCE_ACCURACY_VALUE',
'Maximum model space distance between geometric entities at asserted c
onnectivities');
#8330=UNCERTAINTY_MEASURE_WITH_UNIT(LENGTH_MEASURE(0.001),#8378,
'DISTANCE_ACCURACY_VALUE',
'Maximum model space distance between geometric entities at asserted c
onnectivities');
#8331=UNCERTAINTY_MEASURE_WITH_UNIT(LENGTH_MEASURE(0.001),#8378,
'DISTANCE_ACCURACY_VALUE',
'Maximum model space distance between geometric entities at asserted c
onnectivities');
#8332=UNCERTAINTY_MEASURE_WITH_UNIT(LENGTH_MEASURE(0.001),#8378,
'DISTANCE_ACCURACY_VALUE',
'Maximum model space distance between geometric entities at asserted c
onnectivities');
#8333=UNCERTAINTY_MEASURE_WITH_UNIT(LENGTH_MEASURE(0.001),#8378,
'DISTANCE_ACCURACY_VALUE',
'Maximum model space distance between geometric entities at asserted c
onnectivities');
#8334=UNCERTAINTY_MEASURE_WITH_UNIT(LENGTH_MEASURE(0.001),#8378,
'DISTANCE_ACCURACY_VALUE',
'Maximum model space distance between geometric entities at asserted c
onnectivities');
#8335=UNCERTAINTY_MEASURE_WITH_UNIT(LENGTH_MEASURE(0.001),#8378,
'DISTANCE_ACCURACY_VALUE',
'Maximum model space distance between geometric entities at asserted c
onnectivities');
#8336=UNCERTAINTY_MEASURE_WITH_UNIT(LENGTH_MEASURE(0.001),#8378,
'DISTANCE_ACCURACY_VALUE',
'Maximum model space distance between geometric entities at asserted c
onnectivities');
#8337=UNCERTAINTY_MEASURE_WITH_UNIT(LENGTH_MEASURE(0.001),#8378,
'DISTANCE_ACCURACY_VALUE',
'Maximum model space distance between geometric entities at asserted c
onnectivities');
#8338=UNCERTAINTY_MEASURE_WITH_UNIT(LENGTH_MEASURE(0.001),#8378,
'DISTANCE_ACCURACY_VALUE',
'Maximum model space distance between geometric entities at asserted c
onnectivities');
#8339=UNCERTAINTY_MEASURE_WITH_UNIT(LENGTH_MEASURE(0.001),#8378,
'DISTANCE_ACCURACY_VALUE',
'Maximum model space distance between geometric entities at asserted c
onnectivities');
#8340=UNCERTAINTY_MEASURE_WITH_UNIT(LENGTH_MEASURE(0.001),#8378,
'DISTANCE_ACCURACY_VALUE',
'Maximum model space distance between geometric entities at asserted c
onnectivities');
#8341=UNCERTAINTY_MEASURE_WITH_UNIT(LENGTH_MEASURE(0.001),#8378,
'DISTANCE_ACCURACY_VALUE',
'Maximum model space distance between geometric entities at asserted c
onnectivities');
#8342=UNCERTAINTY_MEASURE_WITH_UNIT(LENGTH_MEASURE(0.001),#8378,
'DISTANCE_ACCURACY_VALUE',
'Maximum model space distance between geometric entities at asserted c
onnectivities');
#8343=UNCERTAINTY_MEASURE_WITH_UNIT(LENGTH_MEASURE(0.001),#8378,
'DISTANCE_ACCURACY_VALUE',
'Maximum model space distance between geometric entities at asserted c
onnectivities');
#8344=UNCERTAINTY_MEASURE_WITH_UNIT(LENGTH_MEASURE(0.001),#8378,
'DISTANCE_ACCURACY_VALUE',
'Maximum model space distance between geometric entities at asserted c
onnectivities');
#8345=UNCERTAINTY_MEASURE_WITH_UNIT(LENGTH_MEASURE(0.001),#8378,
'DISTANCE_ACCURACY_VALUE',
'Maximum model space distance between geometric entities at asserted c
onnectivities');
#8346=(
GEOMETRIC_REPRESENTATION_CONTEXT(3)
GLOBAL_UNCERTAINTY_ASSIGNED_CONTEXT((#8314))
GLOBAL_UNIT_ASSIGNED_CONTEXT((#8378,#8380,#8381))
REPRESENTATION_CONTEXT('','3D')
);
#8347=(
GEOMETRIC_REPRESENTATION_CONTEXT(3)
GLOBAL_UNCERTAINTY_ASSIGNED_CONTEXT((#8315))
GLOBAL_UNIT_ASSIGNED_CONTEXT((#8378,#8380,#8381))
REPRESENTATION_CONTEXT('','3D')
);
#8348=(
GEOMETRIC_REPRESENTATION_CONTEXT(3)
GLOBAL_UNCERTAINTY_ASSIGNED_CONTEXT((#8316))
GLOBAL_UNIT_ASSIGNED_CONTEXT((#8378,#8380,#8381))
REPRESENTATION_CONTEXT('','3D')
);
#8349=(
GEOMETRIC_REPRESENTATION_CONTEXT(3)
GLOBAL_UNCERTAINTY_ASSIGNED_CONTEXT((#8317))
GLOBAL_UNIT_ASSIGNED_CONTEXT((#8378,#8380,#8381))
REPRESENTATION_CONTEXT('','3D')
);
#8350=(
GEOMETRIC_REPRESENTATION_CONTEXT(3)
GLOBAL_UNCERTAINTY_ASSIGNED_CONTEXT((#8318))
GLOBAL_UNIT_ASSIGNED_CONTEXT((#8378,#8380,#8381))
REPRESENTATION_CONTEXT('','3D')
);
#8351=(
GEOMETRIC_REPRESENTATION_CONTEXT(3)
GLOBAL_UNCERTAINTY_ASSIGNED_CONTEXT((#8319))
GLOBAL_UNIT_ASSIGNED_CONTEXT((#8378,#8380,#8381))
REPRESENTATION_CONTEXT('','3D')
);
#8352=(
GEOMETRIC_REPRESENTATION_CONTEXT(3)
GLOBAL_UNCERTAINTY_ASSIGNED_CONTEXT((#8320))
GLOBAL_UNIT_ASSIGNED_CONTEXT((#8378,#8380,#8381))
REPRESENTATION_CONTEXT('','3D')
);
#8353=(
GEOMETRIC_REPRESENTATION_CONTEXT(3)
GLOBAL_UNCERTAINTY_ASSIGNED_CONTEXT((#8321))
GLOBAL_UNIT_ASSIGNED_CONTEXT((#8378,#8380,#8381))
REPRESENTATION_CONTEXT('','3D')
);
#8354=(
GEOMETRIC_REPRESENTATION_CONTEXT(3)
GLOBAL_UNCERTAINTY_ASSIGNED_CONTEXT((#8322))
GLOBAL_UNIT_ASSIGNED_CONTEXT((#8378,#8380,#8381))
REPRESENTATION_CONTEXT('','3D')
);
#8355=(
GEOMETRIC_REPRESENTATION_CONTEXT(3)
GLOBAL_UNCERTAINTY_ASSIGNED_CONTEXT((#8323))
GLOBAL_UNIT_ASSIGNED_CONTEXT((#8378,#8380,#8381))
REPRESENTATION_CONTEXT('','3D')
);
#8356=(
GEOMETRIC_REPRESENTATION_CONTEXT(3)
GLOBAL_UNCERTAINTY_ASSIGNED_CONTEXT((#8324))
GLOBAL_UNIT_ASSIGNED_CONTEXT((#8378,#8380,#8381))
REPRESENTATION_CONTEXT('','3D')
);
#8357=(
GEOMETRIC_REPRESENTATION_CONTEXT(3)
GLOBAL_UNCERTAINTY_ASSIGNED_CONTEXT((#8325))
GLOBAL_UNIT_ASSIGNED_CONTEXT((#8378,#8380,#8381))
REPRESENTATION_CONTEXT('','3D')
);
#8358=(
GEOMETRIC_REPRESENTATION_CONTEXT(3)
GLOBAL_UNCERTAINTY_ASSIGNED_CONTEXT((#8326))
GLOBAL_UNIT_ASSIGNED_CONTEXT((#8378,#8380,#8381))
REPRESENTATION_CONTEXT('','3D')
);
#8359=(
GEOMETRIC_REPRESENTATION_CONTEXT(3)
GLOBAL_UNCERTAINTY_ASSIGNED_CONTEXT((#8327))
GLOBAL_UNIT_ASSIGNED_CONTEXT((#8378,#8380,#8381))
REPRESENTATION_CONTEXT('','3D')
);
#8360=(
GEOMETRIC_REPRESENTATION_CONTEXT(3)
GLOBAL_UNCERTAINTY_ASSIGNED_CONTEXT((#8328))
GLOBAL_UNIT_ASSIGNED_CONTEXT((#8378,#8380,#8381))
REPRESENTATION_CONTEXT('','3D')
);
#8361=(
GEOMETRIC_REPRESENTATION_CONTEXT(3)
GLOBAL_UNCERTAINTY_ASSIGNED_CONTEXT((#8329))
GLOBAL_UNIT_ASSIGNED_CONTEXT((#8378,#8380,#8381))
REPRESENTATION_CONTEXT('','3D')
);
#8362=(
GEOMETRIC_REPRESENTATION_CONTEXT(3)
GLOBAL_UNCERTAINTY_ASSIGNED_CONTEXT((#8330))
GLOBAL_UNIT_ASSIGNED_CONTEXT((#8378,#8380,#8381))
REPRESENTATION_CONTEXT('','3D')
);
#8363=(
GEOMETRIC_REPRESENTATION_CONTEXT(3)
GLOBAL_UNCERTAINTY_ASSIGNED_CONTEXT((#8331))
GLOBAL_UNIT_ASSIGNED_CONTEXT((#8378,#8380,#8381))
REPRESENTATION_CONTEXT('','3D')
);
#8364=(
GEOMETRIC_REPRESENTATION_CONTEXT(3)
GLOBAL_UNCERTAINTY_ASSIGNED_CONTEXT((#8332))
GLOBAL_UNIT_ASSIGNED_CONTEXT((#8378,#8380,#8381))
REPRESENTATION_CONTEXT('','3D')
);
#8365=(
GEOMETRIC_REPRESENTATION_CONTEXT(3)
GLOBAL_UNCERTAINTY_ASSIGNED_CONTEXT((#8333))
GLOBAL_UNIT_ASSIGNED_CONTEXT((#8378,#8380,#8381))
REPRESENTATION_CONTEXT('','3D')
);
#8366=(
GEOMETRIC_REPRESENTATION_CONTEXT(3)
GLOBAL_UNCERTAINTY_ASSIGNED_CONTEXT((#8334))
GLOBAL_UNIT_ASSIGNED_CONTEXT((#8378,#8380,#8381))
REPRESENTATION_CONTEXT('','3D')
);
#8367=(
GEOMETRIC_REPRESENTATION_CONTEXT(3)
GLOBAL_UNCERTAINTY_ASSIGNED_CONTEXT((#8335))
GLOBAL_UNIT_ASSIGNED_CONTEXT((#8378,#8380,#8381))
REPRESENTATION_CONTEXT('','3D')
);
#8368=(
GEOMETRIC_REPRESENTATION_CONTEXT(3)
GLOBAL_UNCERTAINTY_ASSIGNED_CONTEXT((#8336))
GLOBAL_UNIT_ASSIGNED_CONTEXT((#8378,#8380,#8381))
REPRESENTATION_CONTEXT('','3D')
);
#8369=(
GEOMETRIC_REPRESENTATION_CONTEXT(3)
GLOBAL_UNCERTAINTY_ASSIGNED_CONTEXT((#8337))
GLOBAL_UNIT_ASSIGNED_CONTEXT((#8378,#8380,#8381))
REPRESENTATION_CONTEXT('','3D')
);
#8370=(
GEOMETRIC_REPRESENTATION_CONTEXT(3)
GLOBAL_UNCERTAINTY_ASSIGNED_CONTEXT((#8338))
GLOBAL_UNIT_ASSIGNED_CONTEXT((#8378,#8380,#8381))
REPRESENTATION_CONTEXT('','3D')
);
#8371=(
GEOMETRIC_REPRESENTATION_CONTEXT(3)
GLOBAL_UNCERTAINTY_ASSIGNED_CONTEXT((#8339))
GLOBAL_UNIT_ASSIGNED_CONTEXT((#8378,#8380,#8381))
REPRESENTATION_CONTEXT('','3D')
);
#8372=(
GEOMETRIC_REPRESENTATION_CONTEXT(3)
GLOBAL_UNCERTAINTY_ASSIGNED_CONTEXT((#8340))
GLOBAL_UNIT_ASSIGNED_CONTEXT((#8378,#8380,#8381))
REPRESENTATION_CONTEXT('','3D')
);
#8373=(
GEOMETRIC_REPRESENTATION_CONTEXT(3)
GLOBAL_UNCERTAINTY_ASSIGNED_CONTEXT((#8341))
GLOBAL_UNIT_ASSIGNED_CONTEXT((#8378,#8380,#8381))
REPRESENTATION_CONTEXT('','3D')
);
#8374=(
GEOMETRIC_REPRESENTATION_CONTEXT(3)
GLOBAL_UNCERTAINTY_ASSIGNED_CONTEXT((#8342))
GLOBAL_UNIT_ASSIGNED_CONTEXT((#8378,#8380,#8381))
REPRESENTATION_CONTEXT('','3D')
);
#8375=(
GEOMETRIC_REPRESENTATION_CONTEXT(3)
GLOBAL_UNCERTAINTY_ASSIGNED_CONTEXT((#8343))
GLOBAL_UNIT_ASSIGNED_CONTEXT((#8378,#8380,#8381))
REPRESENTATION_CONTEXT('','3D')
);
#8376=(
GEOMETRIC_REPRESENTATION_CONTEXT(3)
GLOBAL_UNCERTAINTY_ASSIGNED_CONTEXT((#8344))
GLOBAL_UNIT_ASSIGNED_CONTEXT((#8378,#8380,#8381))
REPRESENTATION_CONTEXT('','3D')
);
#8377=(
GEOMETRIC_REPRESENTATION_CONTEXT(3)
GLOBAL_UNCERTAINTY_ASSIGNED_CONTEXT((#8345))
GLOBAL_UNIT_ASSIGNED_CONTEXT((#8378,#8380,#8381))
REPRESENTATION_CONTEXT('','3D')
);
#8378=(
LENGTH_UNIT()
NAMED_UNIT(*)
SI_UNIT(.CENTI.,.METRE.)
);
#8379=(
LENGTH_UNIT()
NAMED_UNIT(*)
SI_UNIT($,.METRE.)
);
#8380=(
NAMED_UNIT(*)
PLANE_ANGLE_UNIT()
SI_UNIT($,.RADIAN.)
);
#8381=(
NAMED_UNIT(*)
SI_UNIT($,.STERADIAN.)
SOLID_ANGLE_UNIT()
);
#8382=SHAPE_DEFINITION_REPRESENTATION(#8413,#8497);
#8383=SHAPE_DEFINITION_REPRESENTATION(#8414,#8498);
#8384=SHAPE_DEFINITION_REPRESENTATION(#8415,#8499);
#8385=SHAPE_DEFINITION_REPRESENTATION(#8416,#8500);
#8386=SHAPE_DEFINITION_REPRESENTATION(#8417,#8501);
#8387=SHAPE_DEFINITION_REPRESENTATION(#8418,#8502);
#8388=SHAPE_DEFINITION_REPRESENTATION(#8419,#8503);
#8389=SHAPE_DEFINITION_REPRESENTATION(#8420,#8504);
#8390=SHAPE_DEFINITION_REPRESENTATION(#8421,#8505);
#8391=SHAPE_DEFINITION_REPRESENTATION(#8422,#8506);
#8392=SHAPE_DEFINITION_REPRESENTATION(#8423,#8507);
#8393=SHAPE_DEFINITION_REPRESENTATION(#8424,#8508);
#8394=SHAPE_DEFINITION_REPRESENTATION(#8425,#8509);
#8395=SHAPE_DEFINITION_REPRESENTATION(#8426,#8510);
#8396=SHAPE_DEFINITION_REPRESENTATION(#8427,#8511);
#8397=SHAPE_DEFINITION_REPRESENTATION(#8428,#8512);
#8398=SHAPE_DEFINITION_REPRESENTATION(#8429,#8513);
#8399=SHAPE_DEFINITION_REPRESENTATION(#8430,#8514);
#8400=SHAPE_DEFINITION_REPRESENTATION(#8433,#8515);
#8401=SHAPE_DEFINITION_REPRESENTATION(#8434,#8516);
#8402=SHAPE_DEFINITION_REPRESENTATION(#8469,#8517);
#8403=SHAPE_DEFINITION_REPRESENTATION(#8470,#8518);
#8404=SHAPE_DEFINITION_REPRESENTATION(#8471,#8519);
#8405=SHAPE_DEFINITION_REPRESENTATION(#8472,#8520);
#8406=SHAPE_DEFINITION_REPRESENTATION(#8473,#8521);
#8407=SHAPE_DEFINITION_REPRESENTATION(#8474,#8522);
#8408=SHAPE_DEFINITION_REPRESENTATION(#8475,#8523);
#8409=SHAPE_DEFINITION_REPRESENTATION(#8476,#8524);
#8410=SHAPE_DEFINITION_REPRESENTATION(#8477,#8525);
#8411=SHAPE_DEFINITION_REPRESENTATION(#8478,#8526);
#8412=SHAPE_DEFINITION_REPRESENTATION(#8479,#8527);
#8413=PRODUCT_DEFINITION_SHAPE('',$,#8529);
#8414=PRODUCT_DEFINITION_SHAPE('',$,#8530);
#8415=PRODUCT_DEFINITION_SHAPE('',$,#8531);
#8416=PRODUCT_DEFINITION_SHAPE('',$,#8532);
#8417=PRODUCT_DEFINITION_SHAPE('',$,#8533);
#8418=PRODUCT_DEFINITION_SHAPE('',$,#8534);
#8419=PRODUCT_DEFINITION_SHAPE('',$,#8535);
#8420=PRODUCT_DEFINITION_SHAPE('',$,#8536);
#8421=PRODUCT_DEFINITION_SHAPE('',$,#8537);
#8422=PRODUCT_DEFINITION_SHAPE('',$,#8538);
#8423=PRODUCT_DEFINITION_SHAPE('',$,#8539);
#8424=PRODUCT_DEFINITION_SHAPE('',$,#8540);
#8425=PRODUCT_DEFINITION_SHAPE('',$,#8541);
#8426=PRODUCT_DEFINITION_SHAPE('',$,#8542);
#8427=PRODUCT_DEFINITION_SHAPE('',$,#8543);
#8428=PRODUCT_DEFINITION_SHAPE('',$,#8544);
#8429=PRODUCT_DEFINITION_SHAPE('',$,#8545);
#8430=PRODUCT_DEFINITION_SHAPE('',$,#8546);
#8431=PRODUCT_DEFINITION_SHAPE($,$,#170);
#8432=PRODUCT_DEFINITION_SHAPE($,$,#171);
#8433=PRODUCT_DEFINITION_SHAPE('',$,#8547);
#8434=PRODUCT_DEFINITION_SHAPE('',$,#8548);
#8435=PRODUCT_DEFINITION_SHAPE($,$,#172);
#8436=PRODUCT_DEFINITION_SHAPE($,$,#173);
#8437=PRODUCT_DEFINITION_SHAPE($,$,#174);
#8438=PRODUCT_DEFINITION_SHAPE($,$,#175);
#8439=PRODUCT_DEFINITION_SHAPE($,$,#176);
#8440=PRODUCT_DEFINITION_SHAPE($,$,#177);
#8441=PRODUCT_DEFINITION_SHAPE($,$,#178);
#8442=PRODUCT_DEFINITION_SHAPE($,$,#179);
#8443=PRODUCT_DEFINITION_SHAPE($,$,#180);
#8444=PRODUCT_DEFINITION_SHAPE($,$,#181);
#8445=PRODUCT_DEFINITION_SHAPE($,$,#182);
#8446=PRODUCT_DEFINITION_SHAPE($,$,#183);
#8447=PRODUCT_DEFINITION_SHAPE($,$,#184);
#8448=PRODUCT_DEFINITION_SHAPE($,$,#185);
#8449=PRODUCT_DEFINITION_SHAPE($,$,#186);
#8450=PRODUCT_DEFINITION_SHAPE($,$,#187);
#8451=PRODUCT_DEFINITION_SHAPE($,$,#188);
#8452=PRODUCT_DEFINITION_SHAPE($,$,#189);
#8453=PRODUCT_DEFINITION_SHAPE($,$,#190);
#8454=PRODUCT_DEFINITION_SHAPE($,$,#191);
#8455=PRODUCT_DEFINITION_SHAPE($,$,#192);
#8456=PRODUCT_DEFINITION_SHAPE($,$,#193);
#8457=PRODUCT_DEFINITION_SHAPE($,$,#194);
#8458=PRODUCT_DEFINITION_SHAPE($,$,#195);
#8459=PRODUCT_DEFINITION_SHAPE($,$,#196);
#8460=PRODUCT_DEFINITION_SHAPE($,$,#197);
#8461=PRODUCT_DEFINITION_SHAPE($,$,#198);
#8462=PRODUCT_DEFINITION_SHAPE($,$,#199);
#8463=PRODUCT_DEFINITION_SHAPE($,$,#200);
#8464=PRODUCT_DEFINITION_SHAPE($,$,#201);
#8465=PRODUCT_DEFINITION_SHAPE($,$,#202);
#8466=PRODUCT_DEFINITION_SHAPE($,$,#203);
#8467=PRODUCT_DEFINITION_SHAPE($,$,#204);
#8468=PRODUCT_DEFINITION_SHAPE($,$,#205);
#8469=PRODUCT_DEFINITION_SHAPE('',$,#8549);
#8470=PRODUCT_DEFINITION_SHAPE('',$,#8550);
#8471=PRODUCT_DEFINITION_SHAPE('',$,#8551);
#8472=PRODUCT_DEFINITION_SHAPE('',$,#8552);
#8473=PRODUCT_DEFINITION_SHAPE('',$,#8553);
#8474=PRODUCT_DEFINITION_SHAPE('',$,#8554);
#8475=PRODUCT_DEFINITION_SHAPE('',$,#8555);
#8476=PRODUCT_DEFINITION_SHAPE('',$,#8556);
#8477=PRODUCT_DEFINITION_SHAPE('',$,#8557);
#8478=PRODUCT_DEFINITION_SHAPE('',$,#8558);
#8479=PRODUCT_DEFINITION_SHAPE('',$,#8559);
#8480=PRODUCT_DEFINITION_SHAPE($,$,#206);
#8481=PRODUCT_DEFINITION_SHAPE($,$,#207);
#8482=PRODUCT_DEFINITION_SHAPE($,$,#208);
#8483=PRODUCT_DEFINITION_SHAPE($,$,#209);
#8484=PRODUCT_DEFINITION_SHAPE($,$,#210);
#8485=PRODUCT_DEFINITION_SHAPE($,$,#211);
#8486=PRODUCT_DEFINITION_SHAPE($,$,#212);
#8487=PRODUCT_DEFINITION_SHAPE($,$,#213);
#8488=PRODUCT_DEFINITION_SHAPE($,$,#214);
#8489=PRODUCT_DEFINITION_SHAPE($,$,#215);
#8490=PRODUCT_DEFINITION_SHAPE($,$,#216);
#8491=PRODUCT_DEFINITION_SHAPE($,$,#217);
#8492=PRODUCT_DEFINITION_SHAPE($,$,#218);
#8493=PRODUCT_DEFINITION_SHAPE($,$,#219);
#8494=PRODUCT_DEFINITION_SHAPE($,$,#220);
#8495=PRODUCT_DEFINITION_SHAPE($,$,#221);
#8496=PRODUCT_DEFINITION_SHAPE($,$,#222);
#8497=SHAPE_REPRESENTATION('',(#4653,#5146,#5147),#8346);
#8498=SHAPE_REPRESENTATION('',(#4654,#4930,#4931,#4932,#4933,#4934,#4935,
#4936,#4937,#4938,#4939,#4940,#4941,#4942,#4943,#4944,#4945,#4946,#4947,
#4948,#4949,#4950,#4951,#4952,#4953,#4954,#4955,#4956,#4957,#4958,#4959,
#4960,#4961,#4962,#4963),#8347);
#8499=SHAPE_REPRESENTATION('',(#4655),#8348);
#8500=SHAPE_REPRESENTATION('',(#4692),#8349);
#8501=SHAPE_REPRESENTATION('',(#4707),#8350);
#8502=SHAPE_REPRESENTATION('',(#4714),#8351);
#8503=SHAPE_REPRESENTATION('',(#4729),#8352);
#8504=SHAPE_REPRESENTATION('',(#4736),#8353);
#8505=SHAPE_REPRESENTATION('',(#4745),#8354);
#8506=SHAPE_REPRESENTATION('',(#4754),#8355);
#8507=SHAPE_REPRESENTATION('',(#4763),#8356);
#8508=SHAPE_REPRESENTATION('',(#4772),#8357);
#8509=SHAPE_REPRESENTATION('',(#4781),#8358);
#8510=SHAPE_REPRESENTATION('',(#4790),#8359);
#8511=SHAPE_REPRESENTATION('',(#4799),#8360);
#8512=SHAPE_REPRESENTATION('',(#4825,#4895,#4896),#8361);
#8513=SHAPE_REPRESENTATION('',(#4826),#8362);
#8514=SHAPE_REPRESENTATION('',(#4867),#8363);
#8515=SHAPE_REPRESENTATION('',(#4897),#8364);
#8516=SHAPE_REPRESENTATION('',(#4906),#8365);
#8517=SHAPE_REPRESENTATION('',(#4964,#5131,#5132,#5133,#5134,#5135,#5136,
#5137,#5138,#5139,#5140,#5141,#5142,#5143,#5144,#5145),#8366);
#8518=SHAPE_REPRESENTATION('',(#4965),#8367);
#8519=SHAPE_REPRESENTATION('',(#4993),#8368);
#8520=SHAPE_REPRESENTATION('',(#5011),#8369);
#8521=SHAPE_REPRESENTATION('',(#5029),#8370);
#8522=SHAPE_REPRESENTATION('',(#5044),#8371);
#8523=SHAPE_REPRESENTATION('',(#5059),#8372);
#8524=SHAPE_REPRESENTATION('',(#5068),#8373);
#8525=SHAPE_REPRESENTATION('',(#5077),#8374);
#8526=SHAPE_REPRESENTATION('',(#5088),#8375);
#8527=SHAPE_REPRESENTATION('',(#5105),#8376);
#8528=PRODUCT_DEFINITION_CONTEXT('part definition',#8623,'design');
#8529=PRODUCT_DEFINITION('PAT-068',
'PAT-068',#8560,#8528);
#8530=PRODUCT_DEFINITION('Support frame','Support frame',#8561,#8528);
#8531=PRODUCT_DEFINITION('Base rail','Base rail',#8562,#8528);
#8532=PRODUCT_DEFINITION('Cross foot','Cross foot',#8563,#8528);
#8533=PRODUCT_DEFINITION('Bonded foot pad','Bonded foot pad',#8564,#8528);
#8534=PRODUCT_DEFINITION('Cross foot (1)','Cross foot (1)',#8565,#8528);
#8535=PRODUCT_DEFINITION('Bonded foot pad (1)','Bonded foot pad (1)',#8566,
#8528);
#8536=PRODUCT_DEFINITION('Mounting reducer bush',
'Mounting reducer bush',#8567,#8528);
#8537=PRODUCT_DEFINITION('Mounting reducer bush (1)',
'Mounting reducer bush (1)',#8568,#8528);
#8538=PRODUCT_DEFINITION('Mounting reducer bush (2)',
'Mounting reducer bush (2)',#8569,#8528);
#8539=PRODUCT_DEFINITION('Mounting reducer bush (3)',
'Mounting reducer bush (3)',#8570,#8528);
#8540=PRODUCT_DEFINITION('Mounting reducer bush (4)',
'Mounting reducer bush (4)',#8571,#8528);
#8541=PRODUCT_DEFINITION('Mounting reducer bush (5)',
'Mounting reducer bush (5)',#8572,#8528);
#8542=PRODUCT_DEFINITION('Flat Washer - M6','Flat Washer - M6',#8573,#8528);
#8543=PRODUCT_DEFINITION('Cap Screw - M6x25','Cap Screw - M6x25',#8574,
#8528);
#8544=PRODUCT_DEFINITION('Pillow Block Bearing - 20 mm Bore',
'Pillow Block Bearing - 20 mm Bore',#8575,#8528);
#8545=PRODUCT_DEFINITION('Housing','Housing',#8576,#8528);
#8546=PRODUCT_DEFINITION('Insert bearing','Insert bearing',#8577,#8528);
#8547=PRODUCT_DEFINITION('Flat Washer - M8','Flat Washer - M8',#8578,#8528);
#8548=PRODUCT_DEFINITION('M8x25 Bolt','M8x25 Bolt',#8579,#8528);
#8549=PRODUCT_DEFINITION('Keyed shaft','Keyed shaft',#8580,#8528);
#8550=PRODUCT_DEFINITION('Main shaft','Main shaft',#8581,#8528);
#8551=PRODUCT_DEFINITION('Drive hub','Drive hub',#8582,#8528);
#8552=PRODUCT_DEFINITION('Drive hub (1)','Drive hub (1)',#8583,#8528);
#8553=PRODUCT_DEFINITION('End collar','End collar',#8584,#8528);
#8554=PRODUCT_DEFINITION('End collar (1)','End collar (1)',#8585,#8528);
#8555=PRODUCT_DEFINITION('Shaft end disc','Shaft end disc',#8586,#8528);
#8556=PRODUCT_DEFINITION('Shaft end disc (1)','Shaft end disc (1)',#8587,
#8528);
#8557=PRODUCT_DEFINITION('Key 6x6x20','Key 6x6x20',#8588,#8528);
#8558=PRODUCT_DEFINITION('Socket Set Screw - M5x8',
'Socket Set Screw - M5x8',#8589,#8528);
#8559=PRODUCT_DEFINITION('Cap Screw - M5x20','Cap Screw - M5x20',#8590,
#8528);
#8560=PRODUCT_DEFINITION_FORMATION('',$,#8625);
#8561=PRODUCT_DEFINITION_FORMATION('',$,#8626);
#8562=PRODUCT_DEFINITION_FORMATION('',$,#8627);
#8563=PRODUCT_DEFINITION_FORMATION('',$,#8628);
#8564=PRODUCT_DEFINITION_FORMATION('',$,#8629);
#8565=PRODUCT_DEFINITION_FORMATION('',$,#8630);
#8566=PRODUCT_DEFINITION_FORMATION('',$,#8631);
#8567=PRODUCT_DEFINITION_FORMATION('',$,#8632);
#8568=PRODUCT_DEFINITION_FORMATION('',$,#8633);
#8569=PRODUCT_DEFINITION_FORMATION('',$,#8634);
#8570=PRODUCT_DEFINITION_FORMATION('',$,#8635);
#8571=PRODUCT_DEFINITION_FORMATION('',$,#8636);
#8572=PRODUCT_DEFINITION_FORMATION('',$,#8637);
#8573=PRODUCT_DEFINITION_FORMATION('',$,#8638);
#8574=PRODUCT_DEFINITION_FORMATION('',$,#8639);
#8575=PRODUCT_DEFINITION_FORMATION('',$,#8640);
#8576=PRODUCT_DEFINITION_FORMATION('',$,#8641);
#8577=PRODUCT_DEFINITION_FORMATION('',$,#8642);
#8578=PRODUCT_DEFINITION_FORMATION('',$,#8643);
#8579=PRODUCT_DEFINITION_FORMATION('',$,#8644);
#8580=PRODUCT_DEFINITION_FORMATION('',$,#8645);
#8581=PRODUCT_DEFINITION_FORMATION('',$,#8646);
#8582=PRODUCT_DEFINITION_FORMATION('',$,#8647);
#8583=PRODUCT_DEFINITION_FORMATION('',$,#8648);
#8584=PRODUCT_DEFINITION_FORMATION('',$,#8649);
#8585=PRODUCT_DEFINITION_FORMATION('',$,#8650);
#8586=PRODUCT_DEFINITION_FORMATION('',$,#8651);
#8587=PRODUCT_DEFINITION_FORMATION('',$,#8652);
#8588=PRODUCT_DEFINITION_FORMATION('',$,#8653);
#8589=PRODUCT_DEFINITION_FORMATION('',$,#8654);
#8590=PRODUCT_DEFINITION_FORMATION('',$,#8655);
#8591=PRODUCT_RELATED_PRODUCT_CATEGORY('PAT-068','PAT-068',(#8625));
#8592=PRODUCT_RELATED_PRODUCT_CATEGORY('Support frame','Support frame',
(#8626));
#8593=PRODUCT_RELATED_PRODUCT_CATEGORY('Base rail','Base rail',(#8627));
#8594=PRODUCT_RELATED_PRODUCT_CATEGORY('Cross foot','Cross foot',(#8628));
#8595=PRODUCT_RELATED_PRODUCT_CATEGORY('Bonded foot pad',
'Bonded foot pad',(#8629));
#8596=PRODUCT_RELATED_PRODUCT_CATEGORY('Cross foot (1)',
'Cross foot (1)',(#8630));
#8597=PRODUCT_RELATED_PRODUCT_CATEGORY('Bonded foot pad (1)',
'Bonded foot pad (1)',(#8631));
#8598=PRODUCT_RELATED_PRODUCT_CATEGORY('Mounting reducer bush',
'Mounting reducer bush',(#8632));
#8599=PRODUCT_RELATED_PRODUCT_CATEGORY('Mounting reducer bush (1)',
'Mounting reducer bush (1)',(#8633));
#8600=PRODUCT_RELATED_PRODUCT_CATEGORY('Mounting reducer bush (2)',
'Mounting reducer bush (2)',(#8634));
#8601=PRODUCT_RELATED_PRODUCT_CATEGORY('Mounting reducer bush (3)',
'Mounting reducer bush (3)',(#8635));
#8602=PRODUCT_RELATED_PRODUCT_CATEGORY('Mounting reducer bush (4)',
'Mounting reducer bush (4)',(#8636));
#8603=PRODUCT_RELATED_PRODUCT_CATEGORY('Mounting reducer bush (5)',
'Mounting reducer bush (5)',(#8637));
#8604=PRODUCT_RELATED_PRODUCT_CATEGORY('Flat Washer - M6',
'Flat Washer - M6',(#8638));
#8605=PRODUCT_RELATED_PRODUCT_CATEGORY('Cap Screw - M6x25',
'Cap Screw - M6x25',(#8639));
#8606=PRODUCT_RELATED_PRODUCT_CATEGORY(
'Pillow Block Bearing - 20 mm Bore','Pillow Block Bearing - 20 mm Bore',
(#8640));
#8607=PRODUCT_RELATED_PRODUCT_CATEGORY('Housing','Housing',(#8641));
#8608=PRODUCT_RELATED_PRODUCT_CATEGORY('Insert bearing',
'Insert bearing',(#8642));
#8609=PRODUCT_RELATED_PRODUCT_CATEGORY('Flat Washer - M8',
'Flat Washer - M8',(#8643));
#8610=PRODUCT_RELATED_PRODUCT_CATEGORY('M8x25 Bolt','M8x25 Bolt',(#8644));
#8611=PRODUCT_RELATED_PRODUCT_CATEGORY('Keyed shaft','Keyed shaft',(#8645));
#8612=PRODUCT_RELATED_PRODUCT_CATEGORY('Main shaft','Main shaft',(#8646));
#8613=PRODUCT_RELATED_PRODUCT_CATEGORY('Drive hub','Drive hub',(#8647));
#8614=PRODUCT_RELATED_PRODUCT_CATEGORY('Drive hub (1)','Drive hub (1)',
(#8648));
#8615=PRODUCT_RELATED_PRODUCT_CATEGORY('End collar','End collar',(#8649));
#8616=PRODUCT_RELATED_PRODUCT_CATEGORY('End collar (1)',
'End collar (1)',(#8650));
#8617=PRODUCT_RELATED_PRODUCT_CATEGORY('Shaft end disc',
'Shaft end disc',(#8651));
#8618=PRODUCT_RELATED_PRODUCT_CATEGORY('Shaft end disc (1)',
'Shaft end disc (1)',(#8652));
#8619=PRODUCT_RELATED_PRODUCT_CATEGORY('Key 6x6x20','Key 6x6x20',(#8653));
#8620=PRODUCT_RELATED_PRODUCT_CATEGORY('Socket Set Screw - M5x8',
'Socket Set Screw - M5x8',(#8654));
#8621=PRODUCT_RELATED_PRODUCT_CATEGORY('Cap Screw - M5x20',
'Cap Screw - M5x20',(#8655));
#8622=APPLICATION_PROTOCOL_DEFINITION('international standard',
'automotive_design',2009,#8623);
#8623=APPLICATION_CONTEXT(
'Core Data for Automotive Mechanical Design Process');
#8624=PRODUCT_CONTEXT('part definition',#8623,'mechanical');
#8625=PRODUCT('PAT-068','PAT-068',
'PAT-068',(#8624));
#8626=PRODUCT('Support frame','Support frame','Support frame',(#8624));
#8627=PRODUCT('Base rail','Base rail','Base rail',(#8624));
#8628=PRODUCT('Cross foot','Cross foot','Cross foot',(#8624));
#8629=PRODUCT('Bonded foot pad','Bonded foot pad','Bonded foot pad',(#8624));
#8630=PRODUCT('Cross foot (1)','Cross foot (1)','Cross foot (1)',(#8624));
#8631=PRODUCT('Bonded foot pad (1)','Bonded foot pad (1)',
'Bonded foot pad (1)',(#8624));
#8632=PRODUCT('Mounting reducer bush','Mounting reducer bush',
'Mounting reducer bush',(#8624));
#8633=PRODUCT('Mounting reducer bush (1)','Mounting reducer bush (1)',
'Mounting reducer bush (1)',(#8624));
#8634=PRODUCT('Mounting reducer bush (2)','Mounting reducer bush (2)',
'Mounting reducer bush (2)',(#8624));
#8635=PRODUCT('Mounting reducer bush (3)','Mounting reducer bush (3)',
'Mounting reducer bush (3)',(#8624));
#8636=PRODUCT('Mounting reducer bush (4)','Mounting reducer bush (4)',
'Mounting reducer bush (4)',(#8624));
#8637=PRODUCT('Mounting reducer bush (5)','Mounting reducer bush (5)',
'Mounting reducer bush (5)',(#8624));
#8638=PRODUCT('Flat Washer - M6','Flat Washer - M6','Flat Washer - M6',
(#8624));
#8639=PRODUCT('Cap Screw - M6x25','Cap Screw - M6x25',
'Cap Screw - M6x25',(#8624));
#8640=PRODUCT('Pillow Block Bearing - 20 mm Bore',
'Pillow Block Bearing - 20 mm Bore','Pillow Block Bearing - 20 mm Bore',
(#8624));
#8641=PRODUCT('Housing','Housing','Housing',(#8624));
#8642=PRODUCT('Insert bearing','Insert bearing','Insert bearing',(#8624));
#8643=PRODUCT('Flat Washer - M8','Flat Washer - M8','Flat Washer - M8',
(#8624));
#8644=PRODUCT('M8x25 Bolt','M8x25 Bolt','M8x25 Bolt',(#8624));
#8645=PRODUCT('Keyed shaft','Keyed shaft','Keyed shaft',(#8624));
#8646=PRODUCT('Main shaft','Main shaft','Main shaft',(#8624));
#8647=PRODUCT('Drive hub','Drive hub','Drive hub',(#8624));
#8648=PRODUCT('Drive hub (1)','Drive hub (1)','Drive hub (1)',(#8624));
#8649=PRODUCT('End collar','End collar','End collar',(#8624));
#8650=PRODUCT('End collar (1)','End collar (1)','End collar (1)',(#8624));
#8651=PRODUCT('Shaft end disc','Shaft end disc','Shaft end disc',(#8624));
#8652=PRODUCT('Shaft end disc (1)','Shaft end disc (1)','Shaft end disc (1)',
(#8624));
#8653=PRODUCT('Key 6x6x20','Key 6x6x20','Key 6x6x20',(#8624));
#8654=PRODUCT('Socket Set Screw - M5x8','Socket Set Screw - M5x8',
'Socket Set Screw - M5x8',(#8624));
#8655=PRODUCT('Cap Screw - M5x20','Cap Screw - M5x20',
'Cap Screw - M5x20',(#8624));
#8656=PRESENTATION_STYLE_ASSIGNMENT((#8661));
#8657=PRESENTATION_STYLE_ASSIGNMENT((#8662));
#8658=PRESENTATION_STYLE_ASSIGNMENT((#8663));
#8659=PRESENTATION_STYLE_ASSIGNMENT((#8664));
#8660=PRESENTATION_STYLE_ASSIGNMENT((#8665));
#8661=SURFACE_STYLE_USAGE(.BOTH.,#8666);
#8662=SURFACE_STYLE_USAGE(.BOTH.,#8667);
#8663=SURFACE_STYLE_USAGE(.BOTH.,#8668);
#8664=SURFACE_STYLE_USAGE(.BOTH.,#8669);
#8665=SURFACE_STYLE_USAGE(.BOTH.,#8670);
#8666=SURFACE_SIDE_STYLE('',(#8671));
#8667=SURFACE_SIDE_STYLE('',(#8672));
#8668=SURFACE_SIDE_STYLE('',(#8673));
#8669=SURFACE_SIDE_STYLE('',(#8674));
#8670=SURFACE_SIDE_STYLE('',(#8675));
#8671=SURFACE_STYLE_FILL_AREA(#8676);
#8672=SURFACE_STYLE_FILL_AREA(#8677);
#8673=SURFACE_STYLE_FILL_AREA(#8678);
#8674=SURFACE_STYLE_FILL_AREA(#8679);
#8675=SURFACE_STYLE_FILL_AREA(#8680);
#8676=FILL_AREA_STYLE('Steel - Satin',(#8681));
#8677=FILL_AREA_STYLE('CAD Library Painted - Steel gray',(#8682));
#8678=FILL_AREA_STYLE('CAD Library Painted - Deep blue',(#8683));
#8679=FILL_AREA_STYLE('CAD Library Painted - Graphite',(#8684));
#8680=FILL_AREA_STYLE('CAD Library Painted - Engineering blue',(#8685));
#8681=FILL_AREA_STYLE_COLOUR('Steel - Satin',#8686);
#8682=FILL_AREA_STYLE_COLOUR('CAD Library Painted - Steel gray',#8687);
#8683=FILL_AREA_STYLE_COLOUR('CAD Library Painted - Deep blue',#8688);
#8684=FILL_AREA_STYLE_COLOUR('CAD Library Painted - Graphite',#8689);
#8685=FILL_AREA_STYLE_COLOUR('CAD Library Painted - Engineering blue',#8690);
#8686=COLOUR_RGB('Steel - Satin',0.627450980392157,0.627450980392157,0.627450980392157);
#8687=COLOUR_RGB('CAD Library Painted - Steel gray',0.592156862745098,0.631372549019608,
0.67843137254902);
#8688=COLOUR_RGB('CAD Library Painted - Deep blue',0.0784313725490196,0.203921568627451,
0.349019607843137);
#8689=COLOUR_RGB('CAD Library Painted - Graphite',0.168627450980392,0.192156862745098,
0.231372549019608);
#8690=COLOUR_RGB('CAD Library Painted - Engineering blue',0.12156862745098,
0.356862745098039,0.6);
#8691=COLOUR_RGB('Dark Blue',0.08,0.2,0.34);
#8692=FILL_AREA_STYLE_COLOUR('',#8691);
#8693=FILL_AREA_STYLE('',(#8692));
#8694=SURFACE_STYLE_FILL_AREA(#8693);
#8695=SURFACE_SIDE_STYLE('',(#8694));
#8696=SURFACE_STYLE_USAGE(.BOTH.,#8695);
#8697=PRESENTATION_STYLE_ASSIGNMENT((#8696));
#8698=COLOUR_RGB('Light Blue',0.38,0.62,0.78);
#8699=FILL_AREA_STYLE_COLOUR('',#8698);
#8700=FILL_AREA_STYLE('',(#8699));
#8701=SURFACE_STYLE_FILL_AREA(#8700);
#8702=SURFACE_SIDE_STYLE('',(#8701));
#8703=SURFACE_STYLE_USAGE(.BOTH.,#8702);
#8704=PRESENTATION_STYLE_ASSIGNMENT((#8703));
#8705=COLOUR_RGB('Sky Blue',0.24,0.69,0.87);
#8706=FILL_AREA_STYLE_COLOUR('',#8705);
#8707=FILL_AREA_STYLE('',(#8706));
#8708=SURFACE_STYLE_FILL_AREA(#8707);
#8709=SURFACE_SIDE_STYLE('',(#8708));
#8710=SURFACE_STYLE_USAGE(.BOTH.,#8709);
#8711=PRESENTATION_STYLE_ASSIGNMENT((#8710));
#8712=COLOUR_RGB('Grey',0.48,0.52,0.57);
#8713=FILL_AREA_STYLE_COLOUR('',#8712);
#8714=FILL_AREA_STYLE('',(#8713));
#8715=SURFACE_STYLE_FILL_AREA(#8714);
#8716=SURFACE_SIDE_STYLE('',(#8715));
#8717=SURFACE_STYLE_USAGE(.BOTH.,#8716);
#8718=PRESENTATION_STYLE_ASSIGNMENT((#8717));
#8719=COLOUR_RGB('Black',0.12,0.14,0.17);
#8720=FILL_AREA_STYLE_COLOUR('',#8719);
#8721=FILL_AREA_STYLE('',(#8720));
#8722=SURFACE_STYLE_FILL_AREA(#8721);
#8723=SURFACE_SIDE_STYLE('',(#8722));
#8724=SURFACE_STYLE_USAGE(.BOTH.,#8723);
#8725=PRESENTATION_STYLE_ASSIGNMENT((#8724));
#8726=COLOUR_RGB('Off White',0.89,0.88,0.83);
#8727=FILL_AREA_STYLE_COLOUR('',#8726);
#8728=FILL_AREA_STYLE('',(#8727));
#8729=SURFACE_STYLE_FILL_AREA(#8728);
#8730=SURFACE_SIDE_STYLE('',(#8729));
#8731=SURFACE_STYLE_USAGE(.BOTH.,#8730);
#8732=PRESENTATION_STYLE_ASSIGNMENT((#8731));
ENDSEC;
END-ISO-10303-21;
